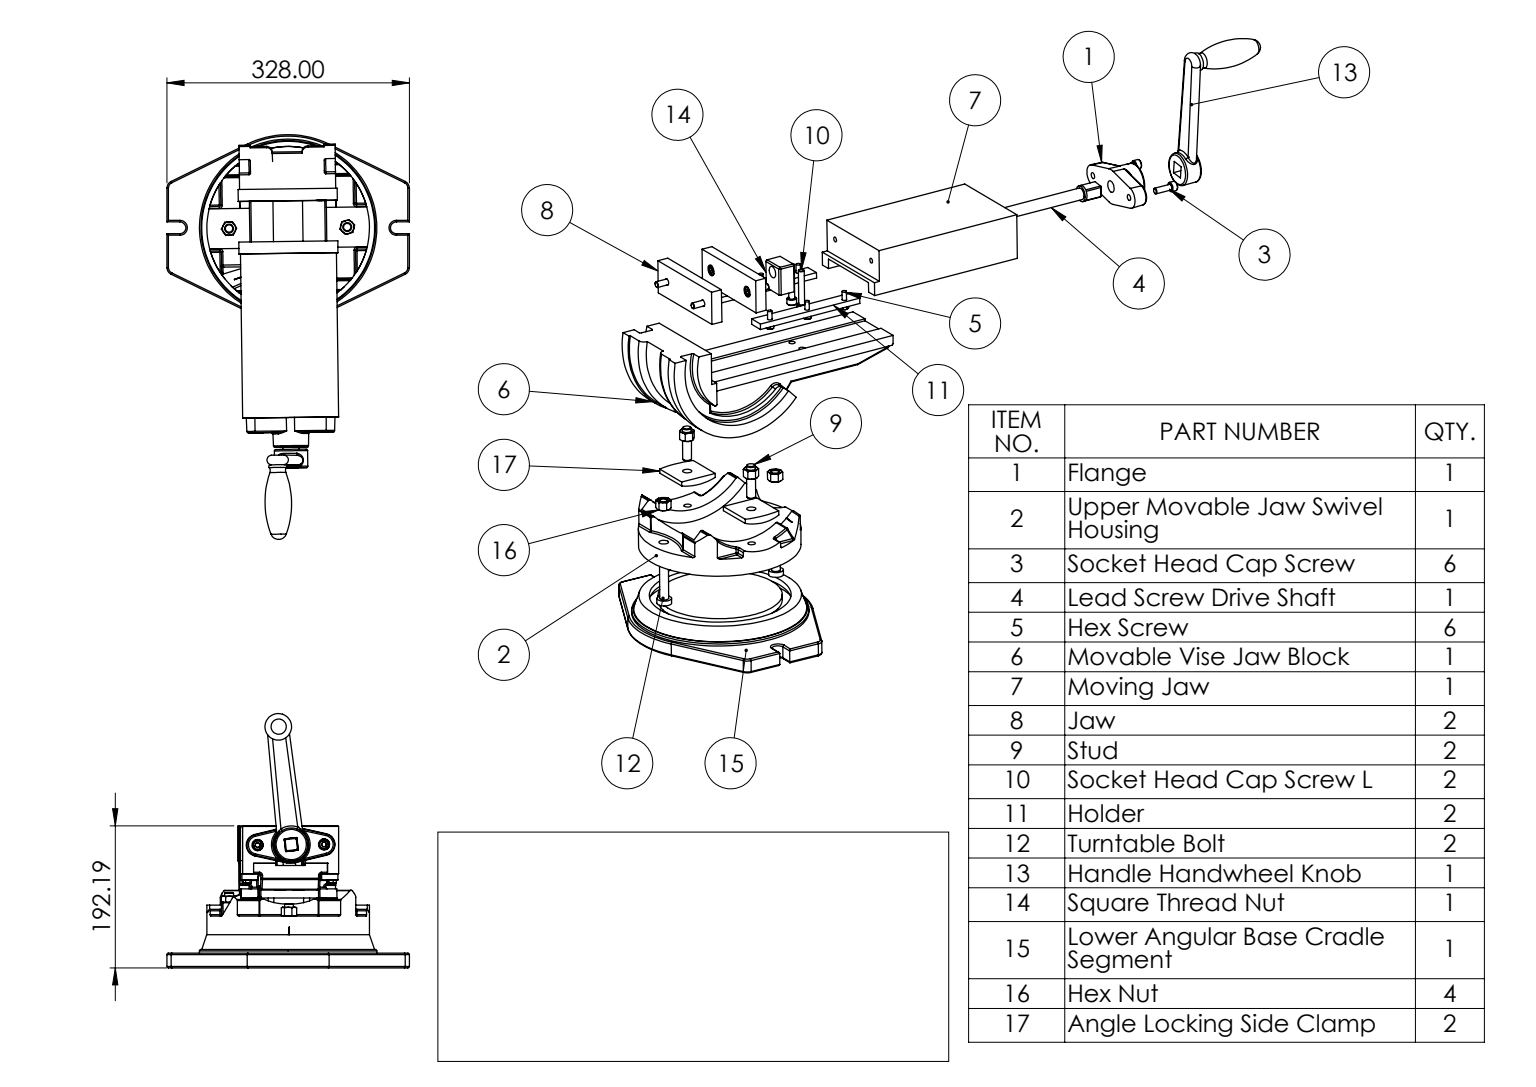
ISO-10303-21;
HEADER;
FILE_DESCRIPTION (('STEP AP214'),
    '1' );
FILE_NAME ('MAS-425',
    '2026-10-09T10:51:02',
    ( '' ),
    ( '' ),
    'SwSTEP 2.0',
    'SolidWorks 2026',
    '' );
FILE_SCHEMA (( 'AUTOMOTIVE_DESIGN' ));
ENDSEC;

DATA;
#1 = ORIENTED_EDGE ( 'NONE', *, *, #17423, .F. ) ;
#2 = EDGE_CURVE ( 'NONE', #15659, #11181, #7452, .T. ) ;
#3 = FACE_BOUND ( 'NONE', #13638, .T. ) ;
#4 = CARTESIAN_POINT ( 'NONE',  ( 8.705884045762138257, 173.3519990577861734, 81.47578913282544022 ) ) ;
#5 = EDGE_LOOP ( 'NONE', ( #8309, #15407, #11959, #15911 ) ) ;
#6 = CARTESIAN_POINT ( 'NONE',  ( -0.1662275214367944787, 327.2814318531398499, 311.3351636502816291 ) ) ;
#7 = LINE ( 'NONE', #21024, #14851 ) ;
#8 = ORIENTED_EDGE ( 'NONE', *, *, #1064, .F. ) ;
#9 = DIRECTION ( 'NONE',  ( 0.01292394549866739996, 0.005513023399721564584, 0.9999012842304692006 ) ) ;
#10 = CARTESIAN_POINT ( 'NONE',  ( -89.78468759032787716, 88.98018858692468314, 52.07678711320818365 ) ) ;
#11 = AXIS2_PLACEMENT_3D ( 'NONE', #11203, #9587, #5900 ) ;
#12 = VERTEX_POINT ( 'NONE', #2655 ) ;
#13 = VECTOR ( 'NONE', #9330, 999.9999999999998863 ) ;
#14 = ORIENTED_EDGE ( 'NONE', *, *, #14466, .T. ) ;
#15 = CARTESIAN_POINT ( 'NONE',  ( -41.94137166082473556, 162.5796238295972671, 273.2086669205137355 ) ) ;
#16 = CARTESIAN_POINT ( 'NONE',  ( -9.107733615807006800, 37.00000000000000711, -96.06569921463757566 ) ) ;
#17 = ORIENTED_EDGE ( 'NONE', *, *, #6536, .F. ) ;
#18 = AXIS2_PLACEMENT_3D ( 'NONE', #16748, #891, #15021 ) ;
#19 = CARTESIAN_POINT ( 'NONE',  ( 83.88156715903123484, 75.05939835648034375, 2.283427986461537440 ) ) ;
#20 = DIRECTION ( 'NONE',  ( 0.9999164797902017066, 6.965998958219365988E-18, -0.01292414190464157356 ) ) ;
#21 = EDGE_LOOP ( 'NONE', ( #14279, #17712, #11551, #2632 ) ) ;
#22 = AXIS2_PLACEMENT_3D ( 'NONE', #15032, #2937, #18572 ) ;
#23 = ORIENTED_EDGE ( 'NONE', *, *, #4860, .T. ) ;
#24 = DIRECTION ( 'NONE',  ( 0.9935244165829104634, 0.1136188085379686713, 0.000000000000000000 ) ) ;
#25 = CARTESIAN_POINT ( 'NONE',  ( -76.57490387278154742, 75.07748563434969924, 4.833641046600559044 ) ) ;
#26 = CARTESIAN_POINT ( 'NONE',  ( -10.01057122740781402, 165.1012737418342056, 308.8014639846969089 ) ) ;
#27 = EDGE_CURVE ( 'NONE', #4135, #17067, #5079, .T. ) ;
#28 = CARTESIAN_POINT ( 'NONE',  ( -105.7487010638476619, 78.91327849199103639, 30.28586431387788380 ) ) ;
#29 = EDGE_CURVE ( 'NONE', #2768, #16051, #13115, .T. ) ;
#30 = DIRECTION ( 'NONE',  ( 0.9909299940865187173, -0.1338359446631173233, -0.01207007604876291287 ) ) ;
#31 = CARTESIAN_POINT ( 'NONE',  ( -56.85751309718151703, 126.2713511641368171, 50.07958431720155090 ) ) ;
#32 = EDGE_CURVE ( 'NONE', #7434, #9119, #18827, .T. ) ;
#33 = AXIS2_PLACEMENT_3D ( 'NONE', #9862, #17006, #490 ) ;
#34 = DIRECTION ( 'NONE',  ( -7.125109674081160920E-05, 0.9999848031710253382, -0.005512562950849312846 ) ) ;
#35 = ORIENTED_EDGE ( 'NONE', *, *, #1256, .T. ) ;
#36 = VECTOR ( 'NONE', #11049, 1000.000000000000000 ) ;
#37 = DIRECTION ( 'NONE',  ( 6.641024085592512675E-15, -1.000000000000000000, 3.383900228611897455E-15 ) ) ;
#38 = ORIENTED_EDGE ( 'NONE', *, *, #21148, .T. ) ;
#39 = ORIENTED_EDGE ( 'NONE', *, *, #19350, .F. ) ;
#40 = UNCERTAINTY_MEASURE_WITH_UNIT (LENGTH_MEASURE( 1.000000000000000082E-05 ), #13566, 'distance_accuracy_value', 'NONE');
#41 = CARTESIAN_POINT ( 'NONE',  ( 15.61516006123881795, 188.4668067408832144, 308.5202341143809690 ) ) ;
#42 = AXIS2_PLACEMENT_3D ( 'NONE', #16731, #4517, #8084 ) ;
#43 = AXIS2_PLACEMENT_3D ( 'NONE', #10674, #12520, #10452 ) ;
#44 = VERTEX_POINT ( 'NONE', #20325 ) ;
#45 = DIRECTION ( 'NONE',  ( -0.7161863329816251511, -0.003898296230782347539, -0.6978982302147140881 ) ) ;
#46 = ADVANCED_BREP_SHAPE_REPRESENTATION ( '', ( #9964, #6292 ), #9601 ) ;
#47 = DIRECTION ( 'NONE',  ( 0.01292394549866738782, 0.005513023399720468239, 0.9999012842304692006 ) ) ;
#48 = CARTESIAN_POINT ( 'NONE',  ( -5.718390838975437873, 144.0378302125689629, 276.6767821598265300 ) ) ;
#49 = DIRECTION ( 'NONE',  ( -0.7944560844389300103, 0.000000000000000000, -0.6073216033519338586 ) ) ;
#50 = AXIS2_PLACEMENT_3D ( 'NONE', #20682, #18849, #13474 ) ;
#51 = CARTESIAN_POINT ( 'NONE',  ( -93.23587179807654479, 72.00000000000000000, -30.79757858250320979 ) ) ;
#52 = CARTESIAN_POINT ( 'NONE',  ( 13.04681478898882219, 190.3009582326741622, 320.8498813576193243 ) ) ;
#53 = CARTESIAN_POINT ( 'NONE',  ( 83.22761354253117361, 75.14843460673597519, -6.385946070498853544 ) ) ;
#54 = VECTOR ( 'NONE', #20690, 999.9999999999998863 ) ;
#55 = CARTESIAN_POINT ( 'NONE',  ( 19.35063451732290929, 183.1639393726175058, 309.5798762404240847 ) ) ;
#56 = CARTESIAN_POINT ( 'NONE',  ( -66.42677970909001317, 189.3893605493459233, -109.9672025422466959 ) ) ;
#57 = CARTESIAN_POINT ( 'NONE',  ( 1.364373935098378649E-14, 105.0000000000000000, -9.836450281572198869E-15 ) ) ;
#58 = EDGE_CURVE ( 'NONE', #6274, #3568, #1285, .T. ) ;
#59 = CARTESIAN_POINT ( 'NONE',  ( 93.17671387018316409, 79.04398536104964990, 26.22064129356684958 ) ) ;
#60 = SHAPE_REPRESENTATION_RELATIONSHIP ( 'NONE' , 'NONE' ,  #16508, #4953 ) ;
#61 = AXIS2_PLACEMENT_3D ( 'NONE', #18338, #21644, #15030 ) ;
#62 = EDGE_CURVE ( 'NONE', #12374, #18464, #11714, .T. ) ;
#63 = CARTESIAN_POINT ( 'NONE',  ( -8.812762866403248907, 186.1645115285507188, 321.8620257335252859 ) ) ;
#64 = DIRECTION ( 'NONE',  ( 0.9934404589540163366, 0.1135548637187051291, -0.01346653032743023830 ) ) ;
#65 = EDGE_LOOP ( 'NONE', ( #10795, #9717, #10945, #15498 ) ) ;
#67 = CARTESIAN_POINT ( 'NONE',  ( -92.91045972105430906, 79.04398536109844997, -26.22408268756080929 ) ) ;
#66 = VECTOR ( 'NONE', #9860, 1000.000000000000114 ) ;
#68 = EDGE_LOOP ( 'NONE', ( #15099, #11264, #5620 ) ) ;
#69 = VECTOR ( 'NONE', #9378, 999.9999999999998863 ) ;
#70 = VECTOR ( 'NONE', #5389, 1000.000000000000000 ) ;
#71 = CARTESIAN_POINT ( 'NONE',  ( -69.75324274910623501, 70.27959272172267902, -85.05633583411399457 ) ) ;
#72 = EDGE_CURVE ( 'NONE', #164, #20449, #17392, .T. ) ;
#73 = CARTESIAN_POINT ( 'NONE',  ( -37.87284078821844702, 165.3754468158257112, 244.8283704289042362 ) ) ;
#74 = ORIENTED_EDGE ( 'NONE', *, *, #20006, .F. ) ;
#75 = DIRECTION ( 'NONE',  ( 0.9999164797902018176, 2.001050586498093021E-22, -0.01292414190464117804 ) ) ;
#76 = CARTESIAN_POINT ( 'NONE',  ( 51.43549903698339421, 154.9275132768233618, 276.0443355225219761 ) ) ;
#77 = DIRECTION ( 'NONE',  ( 0.000000000000000000, 0.000000000000000000, -1.000000000000000000 ) ) ;
#78 = EDGE_CURVE ( 'NONE', #11089, #8677, #1606, .T. ) ;
#79 = ORIENTED_EDGE ( 'NONE', *, *, #13431, .F. ) ;
#80 = FACE_BOUND ( 'NONE', #4943, .T. ) ;
#81 = ORIENTED_EDGE ( 'NONE', *, *, #8487, .T. ) ;
#82 = AXIS2_PLACEMENT_3D ( 'NONE', #13509, #3038, #10060 ) ;
#83 = DIRECTION ( 'NONE',  ( 0.000000000000000000, -1.000000000000000000, 0.000000000000000000 ) ) ;
#84 = VECTOR ( 'NONE', #2049, 1000.000000000000114 ) ;
#85 = PRESENTATION_LAYER_ASSIGNMENT (  '', '', ( #9989 ) ) ;
#86 = CARTESIAN_POINT ( 'NONE',  ( 70.93357090261925180, 91.46354453597338363, 84.07396062241133450 ) ) ;
#87 = CARTESIAN_POINT ( 'NONE',  ( -8.855655583235034101, 185.7709171679380802, 321.2465429934534313 ) ) ;
#88 = DIRECTION ( 'NONE',  ( 0.000000000000000000, 1.000000000000000000, 0.000000000000000000 ) ) ;
#89 = LINE ( 'NONE', #16195, #5542 ) ;
#90 = ORIENTED_EDGE ( 'NONE', *, *, #19194, .F. ) ;
#91 = EDGE_CURVE ( 'NONE', #4221, #20506, #7354, .T. ) ;
#92 = DIRECTION ( 'NONE',  ( 0.9934404589540164476, 0.1135548637187057258, -0.01346653032743022095 ) ) ;
#93 = EDGE_CURVE ( 'NONE', #564, #16051, #11405, .T. ) ;
#94 = CARTESIAN_POINT ( 'NONE',  ( 87.98413419613014241, 100.6041916471018851, -66.02114910964037620 ) ) ;
#95 = CIRCLE ( 'NONE', #9269, 21.67179167071592261 ) ;
#96 = CARTESIAN_POINT ( 'NONE',  ( -45.67464185259402853, 168.2105890667581605, -51.90496219196452188 ) ) ;
#97 = CARTESIAN_POINT ( 'NONE',  ( -15.45047209318716419, 177.9595801977488634, 312.9923267615550344 ) ) ;
#98 = B_SPLINE_CURVE_WITH_KNOTS ( 'NONE', 3,
 ( #3660, #13798, #8829, #3553, #7001, #21013, #121, #3202 ),
 .UNSPECIFIED., .F., .F.,
 ( 4, 2, 2, 4 ),
 ( 0.005257893453559988640, 0.006567392922673305836, 0.007876892391786622163, 0.01049589133001326002 ),
 .UNSPECIFIED. ) ;
#99 = VERTEX_POINT ( 'NONE', #7105 ) ;
#100 = B_SPLINE_CURVE_WITH_KNOTS ( 'NONE', 3,
 ( #8667, #13977, #4769, #10088, #15381, #20512, #13534 ),
 .UNSPECIFIED., .F., .F.,
 ( 4, 3, 4 ),
 ( -5.915969516749687466E-08, 0.000000000000000000, 2.978207829266907417E-05 ),
 .UNSPECIFIED. ) ;
#101 = CARTESIAN_POINT ( 'NONE',  ( 17.83180013577688783, 184.4306634807684588, 307.6366520947308345 ) ) ;
#102 = CARTESIAN_POINT ( 'NONE',  ( -0.5772765004791020615, 70.09252763182293222, -80.84070517186570726 ) ) ;
#103 = DIRECTION ( 'NONE',  ( -7.125109674364536131E-05, 0.9999848031710253382, -0.005512562950849706628 ) ) ;
#104 = CIRCLE ( 'NONE', #1575, 11.00000000000000178 ) ;
#105 = CARTESIAN_POINT ( 'NONE',  ( -9.809641362382285124, 82.00000000000000000, -87.34492244913440118 ) ) ;
#106 = EDGE_CURVE ( 'NONE', #7605, #5654, #6985, .T. ) ;
#107 = ITEM_DEFINED_TRANSFORMATION ( 'NONE', 'NONE', #21637,  #6292 ) ;
#108 = DIRECTION ( 'NONE',  ( -0.9999164797902015955, 0.000000000000000000, 0.01292414190464162733 ) ) ;
#109 = DIRECTION ( 'NONE',  ( -0.01292394549866736179, -0.005513023399728320464, -0.9999012842304692006 ) ) ;
#110 = EDGE_CURVE ( 'NONE', #3828, #14649, #15744, .T. ) ;
#111 = CARTESIAN_POINT ( 'NONE',  ( 11.83347885643962982, 174.6861507205185546, 323.4518999165990181 ) ) ;
#112 = DIRECTION ( 'NONE',  ( 2.025474946048326158E-22, -1.000000000000000000, 1.876735158486679638E-22 ) ) ;
#113 = CONICAL_SURFACE ( 'NONE', #10017, 3.399999999999985700, 1.029744258676653201 ) ;
#114 = DIRECTION ( 'NONE',  ( -0.9999164797902015955, -2.001050586450178695E-22, 0.01292414190464131335 ) ) ;
#115 = ORIENTED_EDGE ( 'NONE', *, *, #3028, .T. ) ;
#116 = FACE_OUTER_BOUND ( 'NONE', #21594, .T. ) ;
#117 = CARTESIAN_POINT ( 'NONE',  ( -39.93340742419142941, 174.9483409995870886, 5.410635606648346752 ) ) ;
#118 = EDGE_LOOP ( 'NONE', ( #17233, #4566 ) ) ;
#119 = CARTESIAN_POINT ( 'NONE',  ( -49.95600144165727841, 95.32463374251413768, -43.99660977802226114 ) ) ;
#120 = EDGE_LOOP ( 'NONE', ( #22099, #16462, #18730 ) ) ;
#121 = CARTESIAN_POINT ( 'NONE',  ( -10.95382118728219289, 70.55908004698140701, -92.00507013140023105 ) ) ;
#122 = FACE_OUTER_BOUND ( 'NONE', #5169, .T. ) ;
#123 = AXIS2_PLACEMENT_3D ( 'NONE', #888, #21632, #12956 ) ;
#124 = CIRCLE ( 'NONE', #10026, 112.5000000000000142 ) ;
#125 = EDGE_CURVE ( 'NONE', #4735, #5612, #10337, .T. ) ;
#126 = VERTEX_POINT ( 'NONE', #10448 ) ;
#127 = FACE_BOUND ( 'NONE', #21151, .T. ) ;
#128 = CARTESIAN_POINT ( 'NONE',  ( 0.3194159855789066582, 327.3487718243365521, 314.2597695910868651 ) ) ;
#129 = EDGE_LOOP ( 'NONE', ( #6381, #6169 ) ) ;
#130 = AXIS2_PLACEMENT_3D ( 'NONE', #8032, #9876, #20201 ) ;
#131 = VECTOR ( 'NONE', #1451, 999.9999999999998863 ) ;
#132 = DIRECTION ( 'NONE',  ( 0.01292394549866738782, 0.005513023399720700692, 0.9999012842304693116 ) ) ;
#133 = CARTESIAN_POINT ( 'NONE',  ( -88.16866694100703228, 88.68864517119313007, 52.43947707082220688 ) ) ;
#135 = ORIENTED_EDGE ( 'NONE', *, *, #14584, .T. ) ;
#134 = VERTEX_POINT ( 'NONE', #1493 ) ;
#136 = AXIS2_PLACEMENT_3D ( 'NONE', #9103, #21501, #2221 ) ;
#137 = B_SPLINE_CURVE_WITH_KNOTS ( 'NONE', 3,
 ( #19717, #16214, #455, #4105, #14828, #14494 ),
 .UNSPECIFIED., .F., .F.,
 ( 4, 2, 4 ),
 ( 2.380730968138597170E-07, 0.002629065763328322300, 0.005257893453559830781 ),
 .UNSPECIFIED. ) ;
#138 = EDGE_CURVE ( 'NONE', #1183, #6442, #10411, .T. ) ;
#139 = ORIENTED_EDGE ( 'NONE', *, *, #21705, .T. ) ;
#140 = DIRECTION ( 'NONE',  ( 0.9999164797902015955, 6.965998958219364448E-18, -0.01292414190464157182 ) ) ;
#141 = CARTESIAN_POINT ( 'NONE',  ( 43.08423624159371457, 94.48610424851698042, 82.84014869562157912 ) ) ;
#142 = CARTESIAN_POINT ( 'NONE',  ( 80.59620023633263486, 75.13519862315604314, -6.109066223056235145 ) ) ;
#143 = CARTESIAN_POINT ( 'NONE',  ( -61.67972807482614428, 191.4143309225244707, 257.3032278304543183 ) ) ;
#144 = EDGE_LOOP ( 'NONE', ( #22040, #16025, #1524, #21274, #7268, #9424, #8449, #10368, #9326, #4340 ) ) ;
#145 = CARTESIAN_POINT ( 'NONE',  ( 20.36241020427591053, 184.0347753543214537, 278.2158687833080535 ) ) ;
#146 = ORIENTED_EDGE ( 'NONE', *, *, #11899, .T. ) ;
#147 = DIRECTION ( 'NONE',  ( 0.9909299940865187173, -0.1338359446631173233, -0.01207007604876291287 ) ) ;
#148 = CARTESIAN_POINT ( 'NONE',  ( -65.67129704762463405, 144.7109461922390778, -51.51693412452669918 ) ) ;
#149 = AXIS2_PLACEMENT_3D ( 'NONE', #2906, #22065, #6366 ) ;
#150 = DIRECTION ( 'NONE',  ( -7.125109674118361251E-05, 0.9999848031710253382, -0.005512562950849477644 ) ) ;
#151 = CIRCLE ( 'NONE', #6013, 2.499999999999988010 ) ;
#152 = CARTESIAN_POINT ( 'NONE',  ( -28.12186643111994044, 324.0859723387359850, 311.7141148554663914 ) ) ;
#153 = ORIENTED_EDGE ( 'NONE', *, *, #18129, .F. ) ;
#154 = PLANE ( 'NONE',  #20182 ) ;
#155 = EDGE_CURVE ( 'NONE', #11795, #1627, #509, .T. ) ;
#156 = CARTESIAN_POINT ( 'NONE',  ( -44.49054948644865703, 166.4747265717734308, 273.2201396957804036 ) ) ;
#157 = PLANE ( 'NONE',  #21075 ) ;
#158 = VECTOR ( 'NONE', #9778, 1000.000000000000000 ) ;
#159 = CARTESIAN_POINT ( 'NONE',  ( 105.4334892372614689, 71.72994009789539405, -31.36525700924963544 ) ) ;
#160 = VERTEX_POINT ( 'NONE', #21115 ) ;
#161 = AXIS2_PLACEMENT_3D ( 'NONE', #9912, #15227, #6474 ) ;
#162 = FACE_BOUND ( 'NONE', #20297, .T. ) ;
#163 = VERTEX_POINT ( 'NONE', #8594 ) ;
#164 = VERTEX_POINT ( 'NONE', #8472 ) ;
#165 = VERTEX_POINT ( 'NONE', #15520 ) ;
#166 = CARTESIAN_POINT ( 'NONE',  ( 14.63430001765469868, 189.2724070846429072, 308.1616490980433696 ) ) ;
#167 = VECTOR ( 'NONE', #3527, 999.9999999999998863 ) ;
#168 = VERTEX_POINT ( 'NONE', #19161 ) ;
#169 = EDGE_CURVE ( 'NONE', #21645, #1999, #4525, .T. ) ;
#170 = EDGE_CURVE ( 'NONE', #168, #18579, #18934, .T. ) ;
#171 = CARTESIAN_POINT ( 'NONE',  ( -90.06393689865117835, 72.00000000000000000, 59.85988923254397065 ) ) ;
#172 = EDGE_CURVE ( 'NONE', #2811, #3408, #19534, .T. ) ;
#173 = CARTESIAN_POINT ( 'NONE',  ( -14.82979117956944037, 177.4987173824078468, 90.64024647396865930 ) ) ;
#174 = AXIS2_PLACEMENT_3D ( 'NONE', #13516, #3386, #10402 ) ;
#175 = VECTOR ( 'NONE', #4968, 999.9999999999998863 ) ;
#176 = FACE_OUTER_BOUND ( 'NONE', #6477, .T. ) ;
#177 = CARTESIAN_POINT ( 'NONE',  ( 79.99331838321626265, 102.0000000000000000, -1.033931352371318058 ) ) ;
#178 = CARTESIAN_POINT ( 'NONE',  ( -38.71484115365228007, 95.23700578170286235, 83.13812943312275650 ) ) ;
#179 = CARTESIAN_POINT ( 'NONE',  ( -41.52755568966412625, 166.0426042274538077, 268.7837904884077034 ) ) ;
#180 = DIRECTION ( 'NONE',  ( 0.9999164797902017066, 2.045740421681430110E-15, -0.01292414190464156835 ) ) ;
#181 = CARTESIAN_POINT ( 'NONE',  ( 15.18113699892158763, 188.8369998821271452, 308.3433818295962396 ) ) ;
#182 = CARTESIAN_POINT ( 'NONE',  ( 92.53737097235195108, 79.85828562204582681, 28.87839056718317465 ) ) ;
#183 = DIRECTION ( 'NONE',  ( 7.125109674160325297E-05, -0.9999848031710252272, 0.005512562950849327591 ) ) ;
#184 = ORIENTED_EDGE ( 'NONE', *, *, #10599, .F. ) ;
#185 = CARTESIAN_POINT ( 'NONE',  ( -10.80196055862741211, 113.7230284608895943, 131.4548877534794542 ) ) ;
#186 = DIRECTION ( 'NONE',  ( -0.01292394549866750231, -0.005513023399722823126, -0.9999012842304692006 ) ) ;
#187 = ORIENTED_EDGE ( 'NONE', *, *, #11712, .T. ) ;
#188 = CARTESIAN_POINT ( 'NONE',  ( -92.67786813602107543, 77.16999450923083259, -28.87226322141232870 ) ) ;
#189 = ORIENTED_EDGE ( 'NONE', *, *, #8901, .F. ) ;
#190 = CIRCLE ( 'NONE', #9344, 2.000000000000000000 ) ;
#191 = CARTESIAN_POINT ( 'NONE',  ( 59.65023440614042727, 143.9188730675116688, 165.9879953250834603 ) ) ;
#192 = FACE_OUTER_BOUND ( 'NONE', #4432, .T. ) ;
#193 = CIRCLE ( 'NONE', #21802, 95.00000000000001421 ) ;
#194 = ORIENTED_EDGE ( 'NONE', *, *, #13859, .T. ) ;
#195 = DIRECTION ( 'NONE',  ( -0.9999164797902015955, -8.506845633049209592E-18, 0.01292414190464159611 ) ) ;
#196 = CARTESIAN_POINT ( 'NONE',  ( 45.44350069997184249, 168.6907664596096765, 34.02200722522287180 ) ) ;
#197 = CARTESIAN_POINT ( 'NONE',  ( 1.163172771417732010, 44.99899999999999523, 89.99248318111813205 ) ) ;
#198 = VERTEX_POINT ( 'NONE', #22578 ) ;
#199 = DIRECTION ( 'NONE',  ( 0.01292394549866734098, 0.005513023399720419666, 0.9999012842304692006 ) ) ;
#200 = ORIENTED_EDGE ( 'NONE', *, *, #18910, .T. ) ;
#201 = LINE ( 'NONE', #14344, #11898 ) ;
#202 = CARTESIAN_POINT ( 'NONE',  ( -39.36913080622078809, 72.00000000000000000, 87.51612159803859470 ) ) ;
#203 = CARTESIAN_POINT ( 'NONE',  ( -8.718981069309306164, 185.8769606721263017, 321.2367416126799640 ) ) ;
#204 = CARTESIAN_POINT ( 'NONE',  ( -90.61229378181283778, 77.84360403296375353, 32.30868923918552582 ) ) ;
#205 = PLANE ( 'NONE',  #10305 ) ;
#206 = ORIENTED_EDGE ( 'NONE', *, *, #693, .T. ) ;
#207 = CARTESIAN_POINT ( 'NONE',  ( -60.33297403592508346, 114.2134059809041418, 166.6289436847881689 ) ) ;
#208 = ADVANCED_FACE ( 'NONE', ( #17222 ), #15410, .F. ) ;
#209 = CARTESIAN_POINT ( 'NONE',  ( -16.46732747216173820, 164.3349221900030557, 301.8725943425079095 ) ) ;
#210 = CARTESIAN_POINT ( 'NONE',  ( 15.90349308958513141, 168.0612899129591824, 307.9342904543644863 ) ) ;
#211 = CARTESIAN_POINT ( 'NONE',  ( -13.46841022152523237, 180.7689078494431669, 321.2689861962914506 ) ) ;
#212 = AXIS2_PLACEMENT_3D ( 'NONE', #480, #21365, #21476 ) ;
#213 = CARTESIAN_POINT ( 'NONE',  ( 20.69445389845595784, 181.8968845288082434, 314.6913679966366999 ) ) ;
#214 = EDGE_LOOP ( 'NONE', ( #14788, #8184, #10598, #16060, #20937 ) ) ;
#215 = ADVANCED_FACE ( 'NONE', ( #14014 ), #12056, .T. ) ;
#216 = DIRECTION ( 'NONE',  ( 0.000000000000000000, 1.000000000000000000, -0.000000000000000000 ) ) ;
#217 = CONTEXT_DEPENDENT_SHAPE_REPRESENTATION ( #13531, #16900 ) ;
#218 = CARTESIAN_POINT ( 'NONE',  ( 36.24790013166018099, 94.37751527644310556, 82.16087381192814121 ) ) ;
#219 = EDGE_CURVE ( 'NONE', #11742, #21224, #10193, .T. ) ;
#220 = EDGE_CURVE ( 'NONE', #18203, #7136, #3541, .T. ) ;
#221 = CARTESIAN_POINT ( 'NONE',  ( -17.10066205189340849, 316.2389990861104820, 322.8183011548654804 ) ) ;
#222 = CYLINDRICAL_SURFACE ( 'NONE', #2944, 2.000000000000001776 ) ;
#223 = DIRECTION ( 'NONE',  ( 0.9232306267972774094, 0.000000000000000000, -0.3842462878721227826 ) ) ;
#224 = EDGE_LOOP ( 'NONE', ( #13231, #22623, #16630, #19910 ) ) ;
#225 = EDGE_LOOP ( 'NONE', ( #13563, #14195, #15245 ) ) ;
#226 = CARTESIAN_POINT ( 'NONE',  ( -41.56623493000981284, 72.00000000000000000, -82.46967996629571473 ) ) ;
#227 = PRODUCT_DEFINITION_SHAPE ( 'NONE', 'NONE',  #22690 ) ;
#228 = CARTESIAN_POINT ( 'NONE',  ( -1.163172771417702700, 69.99999999999998579, -89.99248318111824574 ) ) ;
#229 = ORIENTED_EDGE ( 'NONE', *, *, #7447, .T. ) ;
#230 = CARTESIAN_POINT ( 'NONE',  ( 39.42082737383937996, 91.17157287525387233, -83.51645567887783272 ) ) ;
#231 = ORIENTED_EDGE ( 'NONE', *, *, #5950, .F. ) ;
#232 = CARTESIAN_POINT ( 'NONE',  ( 106.2491592972476298, 77.90302844854615216, 28.48020057081471279 ) ) ;
#233 = DIRECTION ( 'NONE',  ( -0.9232306267972774094, 0.000000000000000000, 0.3842462878721227826 ) ) ;
#234 = DIRECTION ( 'NONE',  ( -0.01292394549866745720, -0.005513023399720816918, -0.9999012842304692006 ) ) ;
#235 = EDGE_CURVE ( 'NONE', #9934, #22618, #12029, .T. ) ;
#236 = EDGE_LOOP ( 'NONE', ( #19815, #2984, #795, #12420, #9588 ) ) ;
#237 = DIRECTION ( 'NONE',  ( 0.000000000000000000, 0.000000000000000000, 1.000000000000000000 ) ) ;
#238 = DIRECTION ( 'NONE',  ( 0.01246513159389400598, 0.2641402835564878870, 0.9644037178988087433 ) ) ;
#239 = CARTESIAN_POINT ( 'NONE',  ( 21.90287145686899706, 168.7773271647431841, 315.3565719312696842 ) ) ;
#240 = EDGE_CURVE ( 'NONE', #22376, #21368, #5043, .T. ) ;
#241 = ORIENTED_EDGE ( 'NONE', *, *, #10232, .T. ) ;
#242 = CARTESIAN_POINT ( 'NONE',  ( -29.42617654240078551, 169.3906321239456361, -110.1596432836334856 ) ) ;
#243 = CARTESIAN_POINT ( 'NONE',  ( -89.64611244253616462, 89.06139627483084098, 51.86061978640490366 ) ) ;
#244 = ADVANCED_FACE ( 'NONE', ( #2899 ), #1200, .F. ) ;
#246 = ORIENTED_EDGE ( 'NONE', *, *, #15979, .F. ) ;
#245 = ORIENTED_EDGE ( 'NONE', *, *, #7257, .T. ) ;
#247 = EDGE_CURVE ( 'NONE', #11011, #13307, #20124, .T. ) ;
#248 = ORIENTED_EDGE ( 'NONE', *, *, #8242, .F. ) ;
#249 = DIRECTION ( 'NONE',  ( 0.3101392564284310427, 0.9506461370142480494, -0.009250070373107139796 ) ) ;
#250 = DIRECTION ( 'NONE',  ( 0.01292394549866731669, 0.005513023399720593139, 0.9999012842304692006 ) ) ;
#251 = VERTEX_POINT ( 'NONE', #22395 ) ;
#252 = CARTESIAN_POINT ( 'NONE',  ( 11.11764968563295142, 180.4772689128618879, 86.40582449793498654 ) ) ;
#253 = CARTESIAN_POINT ( 'NONE',  ( -90.15100670864553933, 87.99029836822313655, 53.12346227685477373 ) ) ;
#254 = LINE ( 'NONE', #14055, #10043 ) ;
#255 = ORIENTED_EDGE ( 'NONE', *, *, #12322, .T. ) ;
#256 = CARTESIAN_POINT ( 'NONE',  ( 48.39260390757410590, 174.4164586986524057, 267.9754221921975272 ) ) ;
#257 = ORIENTED_EDGE ( 'NONE', *, *, #16631, .F. ) ;
#258 = CARTESIAN_POINT ( 'NONE',  ( 79.99331838321626265, 54.99999999999999289, -1.033931352371318058 ) ) ;
#259 = DIRECTION ( 'NONE',  ( -0.000000000000000000, -1.000000000000000000, -0.000000000000000000 ) ) ;
#260 = DIRECTION ( 'NONE',  ( -0.9934404589540163366, -0.1135548637187053511, 0.01346653032743023309 ) ) ;
#261 = CARTESIAN_POINT ( 'NONE',  ( -28.28143568398816399, 324.0695986473149901, 312.1786345499324398 ) ) ;
#262 = DIRECTION ( 'NONE',  ( -0.01292394549866739996, -0.005513023399721131770, -0.9999012842304692006 ) ) ;
#263 = CARTESIAN_POINT ( 'NONE',  ( -39.11958398656035030, 107.9174803907495885, 72.42004164600064087 ) ) ;
#264 = DIRECTION ( 'NONE',  ( -7.125109674159588039E-05, 0.9999848031710253382, -0.005512562950848870491 ) ) ;
#265 = CARTESIAN_POINT ( 'NONE',  ( 105.3069082217399597, 70.76149960027359498, -31.78775043357529739 ) ) ;
#266 = ORIENTED_EDGE ( 'NONE', *, *, #3629, .T. ) ;
#267 = ADVANCED_FACE ( 'NONE', ( #15553 ), #14170, .F. ) ;
#268 = DIRECTION ( 'NONE',  ( 0.9232306267972772984, 0.000000000000000000, -0.3842462878721232822 ) ) ;
#269 = EDGE_LOOP ( 'NONE', ( #10049, #17678 ) ) ;
#270 = ORIENTED_EDGE ( 'NONE', *, *, #14726, .F. ) ;
#271 = EDGE_LOOP ( 'NONE', ( #6417, #19362, #17256, #12411 ) ) ;
#272 = UNCERTAINTY_MEASURE_WITH_UNIT (LENGTH_MEASURE( 1.000000000000000082E-05 ), #22042, 'distance_accuracy_value', 'NONE');
#273 = CARTESIAN_POINT ( 'NONE',  ( 19.91213793988244163, 183.5619383714575861, 314.9323046934921422 ) ) ;
#274 = ORIENTED_EDGE ( 'NONE', *, *, #11916, .F. ) ;
#275 = ADVANCED_FACE ( 'NONE', ( #19418 ), #17495, .F. ) ;
#276 = FACE_OUTER_BOUND ( 'NONE', #812, .T. ) ;
#277 = DIRECTION ( 'NONE',  ( 0.9999164797902017066, 2.001050586450178931E-22, -0.01292414190464131508 ) ) ;
#278 = CARTESIAN_POINT ( 'NONE',  ( -91.88175745861167343, 69.99999999999998579, 60.48014731673399069 ) ) ;
#279 = FACE_BOUND ( 'NONE', #1045, .T. ) ;
#280 = CARTESIAN_POINT ( 'NONE',  ( -38.57134427488318806, 95.07266577213218284, 83.30245068639356987 ) ) ;
#281 = DIRECTION ( 'NONE',  ( -0.01292394549866733230, -0.005513023399720419666, -0.9999012842304692006 ) ) ;
#282 = CARTESIAN_POINT ( 'NONE',  ( 76.11837255219295173, 75.12984171660241373, -5.954615140807677953 ) ) ;
#283 = CARTESIAN_POINT ( 'NONE',  ( 19.70626577706693894, 182.8347090725441433, 310.2503944804881826 ) ) ;
#284 = CARTESIAN_POINT ( 'NONE',  ( 90.70439626174579928, 79.29995750804924626, 27.08818539008225912 ) ) ;
#285 = CARTESIAN_POINT ( 'NONE',  ( 90.15711184568685610, 79.46353706204938305, 27.61532001585838714 ) ) ;
#286 = ORIENTED_EDGE ( 'NONE', *, *, #7951, .T. ) ;
#287 =( NAMED_UNIT ( * ) SI_UNIT ( $, .STERADIAN. ) SOLID_ANGLE_UNIT ( ) );
#288 = CIRCLE ( 'NONE', #22624, 0.009999999999999205705 ) ;
#289 = ADVANCED_FACE ( 'NONE', ( #16063 ), #9015, .T. ) ;
#290 = CARTESIAN_POINT ( 'NONE',  ( -9.470826101554981946, 187.1917151187963384, 321.2300099800097541 ) ) ;
#291 = DIRECTION ( 'NONE',  ( 7.125109674160258889E-05, -0.9999848031710252272, 0.005512562950849897447 ) ) ;
#292 = EDGE_CURVE ( 'NONE', #16435, #21883, #7077, .T. ) ;
#293 = ORIENTED_EDGE ( 'NONE', *, *, #12181, .F. ) ;
#294 = DIRECTION ( 'NONE',  ( 0.7069973413461587697, 0.7070960354057281849, -0.01303671902605322945 ) ) ;
#295 = EDGE_LOOP ( 'NONE', ( #16677, #766, #19558, #3200 ) ) ;
#296 = B_SPLINE_CURVE_WITH_KNOTS ( 'NONE', 3,
 ( #20681, #1405, #18731, #13805, #4936, #18621, #1059, #11969, #4819, #17038, #18953, #20788, #17137, #20446, #8179, #13473 ),
 .UNSPECIFIED., .F., .F.,
 ( 4, 2, 2, 2, 2, 2, 2, 4 ),
 ( 0.000000000000000000, 0.0008474927940828290429, 0.001271239191124224699, 0.001694985588165620572, 0.002118731985207016229, 0.002542478382248412102, 0.002966224779289807541, 0.003389971176331203415 ),
 .UNSPECIFIED. ) ;
#297 = VECTOR ( 'NONE', #9208, 1000.000000000000114 ) ;
#298 = EDGE_LOOP ( 'NONE', ( #1646, #5855, #3036, #20103 ) ) ;
#299 = CARTESIAN_POINT ( 'NONE',  ( -5.672696058028124710, 81.44153265534504271, -98.91173476717540325 ) ) ;
#300 = CARTESIAN_POINT ( 'NONE',  ( -1.163172771417702700, 81.97459999999998104, -89.99248318111824574 ) ) ;
#301 = EDGE_LOOP ( 'NONE', ( #15173, #17120, #19580, #5311 ) ) ;
#302 = DIRECTION ( 'NONE',  ( 0.01292394549866740169, 0.005513023399720822990, 0.9999012842304693116 ) ) ;
#303 = VECTOR ( 'NONE', #7071, 999.9999999999998863 ) ;
#304 =( REPRESENTATION_RELATIONSHIP ('NONE','NONE', #11808, #10922 ) REPRESENTATION_RELATIONSHIP_WITH_TRANSFORMATION ( #3089 )SHAPE_REPRESENTATION_RELATIONSHIP( ) );
#305 = DIRECTION ( 'NONE',  ( 0.9506032891036977350, -0.3102281881984299550, -0.01057629388543066158 ) ) ;
#306 = B_SPLINE_CURVE_WITH_KNOTS ( 'NONE', 3,
 ( #21331, #5362, #6982, #1942, #105, #14363 ),
 .UNSPECIFIED., .F., .F.,
 ( 4, 2, 4 ),
 ( 0.009270618776430233909, 0.01189894710419334665, 0.01452727543195645940 ),
 .UNSPECIFIED. ) ;
#307 = VERTEX_POINT ( 'NONE', #5575 ) ;
#308 = CARTESIAN_POINT ( 'NONE',  ( -22.02882225528089322, 319.7347194434814242, 320.5895957426023415 ) ) ;
#309 = VERTEX_POINT ( 'NONE', #21424 ) ;
#310 = CARTESIAN_POINT ( 'NONE',  ( -55.33894950108835076, 126.9191314136037789, 167.5679852142818334 ) ) ;
#311 = DIRECTION ( 'NONE',  ( 0.01292394549866739996, 0.005513023399721131770, 0.9999012842304692006 ) ) ;
#312 = EDGE_LOOP ( 'NONE', ( #22638, #21700, #16864 ) ) ;
#313 = CARTESIAN_POINT ( 'NONE',  ( -10.06383400738342360, 187.4687485412983108, 321.1393786276795481 ) ) ;
#314 = CARTESIAN_POINT ( 'NONE',  ( -91.08520856931303911, 77.44390114805533187, 31.69197020849769686 ) ) ;
#315 = CARTESIAN_POINT ( 'NONE',  ( 67.23655452815148692, 145.1029152106949027, 17.86880078497820179 ) ) ;
#316 = ORIENTED_EDGE ( 'NONE', *, *, #15570, .F. ) ;
#317 = TOROIDAL_SURFACE ( 'NONE', #19007, 12.37020706055087516, 2.000000000000000000 ) ;
#318 = CARTESIAN_POINT ( 'NONE',  ( -13.33381189847107784, 183.5857969768588589, 309.7596506135559480 ) ) ;
#319 = ADVANCED_FACE ( 'NONE', ( #17546 ), #8781, .T. ) ;
#320 = CARTESIAN_POINT ( 'NONE',  ( -41.47069032946998846, 166.0668615304125808, 273.1833561390217824 ) ) ;
#321 = AXIS2_PLACEMENT_3D ( 'NONE', #22086, #7878, #10397 ) ;
#322 = CARTESIAN_POINT ( 'NONE',  ( 18.31365161534814945, 168.3394720871181960, 308.5681747117120608 ) ) ;
#323 = CARTESIAN_POINT ( 'NONE',  ( -14.60451153091767118, 179.2935387600311401, 317.4001766113444774 ) ) ;
#324 = ORIENTED_EDGE ( 'NONE', *, *, #12603, .F. ) ;
#325 = DIRECTION ( 'NONE',  ( 0.01292414190464174703, 0.000000000000000000, 0.9999164797902015955 ) ) ;
#326 =( BOUNDED_SURFACE ( )  B_SPLINE_SURFACE ( 3, 2, ( 
 ( #2487, #894, #11567 ),
 ( #1117, #14687, #22097 ),
 ( #11112, #18134, #9486 ),
 ( #2827, #8113, #7770 ),
 ( #14809, #13081, #4304 ),
 ( #11333, #16646, #14924 ),
 ( #998, #21864, #6160 ),
 ( #13185, #2385, #20151 ),
 ( #18461, #2723, #4540 ),
 ( #9377, #16853, #16751 ),
 ( #15145, #7985, #15025 ),
 ( #21979, #6279, #13305 ),
 ( #6398, #19810, #16411 ),
 ( #10404, #6504, #1347 ),
 ( #4752, #11794, #13518 ),
 ( #6725, #18893, #10288 ),
 ( #3156, #15697, #11911 ),
 ( #15366, #3390, #10171 ) ),
 .UNSPECIFIED., .F., .F., .T. ) 
 B_SPLINE_SURFACE_WITH_KNOTS ( ( 4, 2, 2, 2, 2, 2, 2, 2, 4 ),
 ( 3, 3 ),
 ( 0.002597246120634449582, 0.003399884678228176898, 0.004202523235821904214, 0.005005161793415631097, 0.005807800351009358847, 0.006610438908603086597, 0.007413077466196813479, 0.008215716023790540362, 0.009018354581384268112 ),
 ( 0.000000000000000000, 1.000000000000000000 ),
 .UNSPECIFIED. ) 
 GEOMETRIC_REPRESENTATION_ITEM ( )  RATIONAL_B_SPLINE_SURFACE ( (
 ( 1.000000000000000000, 0.5963808372950818448, 1.000000000000000000),
 ( 1.000000000000000000, 0.5963839598475944026, 1.000000000000000000),
 ( 1.000000000000000000, 0.5970886094881097117, 1.000000000000000000),
 ( 1.000000000000000000, 0.5998681984912884735, 1.000000000000000000),
 ( 1.000000000000000000, 0.6019790828716350406, 1.000000000000000000),
 ( 1.000000000000000000, 0.6074656362385489894, 1.000000000000000000),
 ( 1.000000000000000000, 0.6108290540004600588, 1.000000000000000000),
 ( 1.000000000000000000, 0.6188252630046860991, 1.000000000000000000),
 ( 1.000000000000000000, 0.6234423941984682527, 1.000000000000000000),
 ( 1.000000000000000000, 0.6335838931037546251, 1.000000000000000000),
 ( 1.000000000000000000, 0.6391861101558512503, 1.000000000000000000),
 ( 1.000000000000000000, 0.6512661799274815921, 1.000000000000000000),
 ( 1.000000000000000000, 0.6576333021889211317, 1.000000000000000000),
 ( 1.000000000000000000, 0.6710088154584188391, 1.000000000000000000),
 ( 1.000000000000000000, 0.6780884601156443869, 1.000000000000000000),
 ( 1.000000000000000000, 0.6924279500034885571, 1.000000000000000000),
 ( 1.000000000000000000, 0.6997125326201816264, 1.000000000000000000),
 ( 1.000000000000000000, 0.7071067811865476838, 1.000000000000000000) ) ) 
 REPRESENTATION_ITEM ( '' )  SURFACE ( )  );
#327 = ORIENTED_EDGE ( 'NONE', *, *, #6954, .T. ) ;
#328 = CARTESIAN_POINT ( 'NONE',  ( 11.85964614693714836, 187.7423844643599296, 304.8777488482054423 ) ) ;
#329 = CIRCLE ( 'NONE', #7287, 112.5000000000000284 ) ;
#330 = CARTESIAN_POINT ( 'NONE',  ( -9.841028579513169561, 187.8130746588807938, 321.1594247271215750 ) ) ;
#331 = DIRECTION ( 'NONE',  ( 2.025474946048326158E-22, -1.000000000000000000, 1.876735158486679638E-22 ) ) ;
#332 = VECTOR ( 'NONE', #8959, 1000.000000000000114 ) ;
#333 = DIRECTION ( 'NONE',  ( -0.7070981056135049458, 0.7070960354057279629, 0.005240777737525892203 ) ) ;
#334 = ORIENTED_EDGE ( 'NONE', *, *, #20168, .F. ) ;
#335 = CARTESIAN_POINT ( 'NONE',  ( -66.44851505496320954, 169.3797848675314128, -111.6488252521261160 ) ) ;
#336 = LINE ( 'NONE', #12856, #8327 ) ;
#337 = ORIENTED_EDGE ( 'NONE', *, *, #2949, .T. ) ;
#338 = CARTESIAN_POINT ( 'NONE',  ( -50.59154831888564274, 96.21415597129798414, -45.44386052779758245 ) ) ;
#339 = ORIENTED_EDGE ( 'NONE', *, *, #11190, .F. ) ;
#340 = CARTESIAN_POINT ( 'NONE',  ( -48.94038278341281512, 95.51270090492249665, 82.30370228625183415 ) ) ;
#341 = DIRECTION ( 'NONE',  ( 0.01292394549866738782, 0.005513023399720700692, 0.9999012842304693116 ) ) ;
#342 = DIRECTION ( 'NONE',  ( 0.3101392564284315978, 0.9506461370142478273, -0.009250070373107145000 ) ) ;
#343 = CARTESIAN_POINT ( 'NONE',  ( 11.77442667496907625, 158.9997348699313591, 299.5367818821357560 ) ) ;
#344 = ORIENTED_EDGE ( 'NONE', *, *, #10316, .T. ) ;
#345 = VERTEX_POINT ( 'NONE', #76 ) ;
#346 = CARTESIAN_POINT ( 'NONE',  ( 40.57355171551004958, 108.0982075334647163, 198.8652726751216449 ) ) ;
#347 = CLOSED_SHELL ( 'NONE', ( #16015, #16676, #7875, #358, #5419, #11925, #2214, #215, #20046 ) ) ;
#348 = AXIS2_PLACEMENT_3D ( 'NONE', #1799, #199, #10640 ) ;
#349 = EDGE_CURVE ( 'NONE', #12132, #16568, #18988, .T. ) ;
#350 = CARTESIAN_POINT ( 'NONE',  ( 0.2417370086904135351, 327.3338204178164688, 312.7560729848880214 ) ) ;
#351 = CIRCLE ( 'NONE', #15405, 6.500000000000013323 ) ;
#352 = EDGE_LOOP ( 'NONE', ( #16374, #6015 ) ) ;
#353 = CARTESIAN_POINT ( 'NONE',  ( -42.64894290516974706, 118.1474297122749135, 27.43850586800562752 ) ) ;
#354 = CARTESIAN_POINT ( 'NONE',  ( -89.81089220510853011, 88.95379388444949598, 52.12444704693557895 ) ) ;
#355 = SHAPE_DEFINITION_REPRESENTATION ( #14203, #21889 ) ;
#357 = ORIENTED_EDGE ( 'NONE', *, *, #20567, .F. ) ;
#356 = ORIENTED_EDGE ( 'NONE', *, *, #20168, .T. ) ;
#358 = ADVANCED_FACE ( 'NONE', ( #21968 ), #16637, .T. ) ;
#359 = ORIENTED_EDGE ( 'NONE', *, *, #12423, .F. ) ;
#360 = CARTESIAN_POINT ( 'NONE',  ( -12.86548928906161571, 326.2291019854885121, 410.4442357137708086 ) ) ;
#361 = CARTESIAN_POINT ( 'NONE',  ( -44.25520882077128704, 168.2183454221810734, 273.2074843050344271 ) ) ;
#362 = EDGE_LOOP ( 'NONE', ( #12674, #9127, #10341, #20941, #20495 ) ) ;
#363 = AXIS2_PLACEMENT_3D ( 'NONE', #1584, #20516, #11935 ) ;
#364 = DIRECTION ( 'NONE',  ( -0.000000000000000000, -1.000000000000000000, 0.000000000000000000 ) ) ;
#365 = MECHANICAL_DESIGN_GEOMETRIC_PRESENTATION_REPRESENTATION (  '', ( #14686 ), #5105 ) ;
#366 = DIRECTION ( 'NONE',  ( 7.125109674403838460E-05, -0.9999848031710253382, 0.005512562950847868688 ) ) ;
#367 = VERTEX_POINT ( 'NONE', #15252 ) ;
#368 = EDGE_CURVE ( 'NONE', #10057, #21384, #12802, .T. ) ;
#369 = VERTEX_POINT ( 'NONE', #17174 ) ;
#370 = AXIS2_PLACEMENT_3D ( 'NONE', #9762, #6313, #11942 ) ;
#371 = CARTESIAN_POINT ( 'NONE',  ( -93.21002351426726307, 77.12912189496638860, -28.79774562292281104 ) ) ;
#372 = CARTESIAN_POINT ( 'NONE',  ( -24.73308955485819283, 324.4589790655039110, 308.1131263010046837 ) ) ;
#373 = CARTESIAN_POINT ( 'NONE',  ( 50.34271970654513950, 126.1473081376433214, 26.19246016726700788 ) ) ;
#374 = CYLINDRICAL_SURFACE ( 'NONE', #1941, 2.000000000000001332 ) ;
#375 = DIRECTION ( 'NONE',  ( 0.01292394549866743812, 0.005513023399720639109, 0.9999012842304693116 ) ) ;
#376 = AXIS2_PLACEMENT_3D ( 'NONE', #2393, #7090, #10992 ) ;
#377 = CYLINDRICAL_SURFACE ( 'NONE', #4764, 2.499999999999988010 ) ;
#378 = ADVANCED_FACE ( 'NONE', ( #6928 ), #5321, .T. ) ;
#379 = VERTEX_POINT ( 'NONE', #17766 ) ;
#380 = EDGE_CURVE ( 'NONE', #16237, #5742, #16043, .T. ) ;
#381 = DIRECTION ( 'NONE',  ( 7.125109674160258889E-05, -0.9999848031710252272, 0.005512562950849897447 ) ) ;
#382 = ORIENTED_EDGE ( 'NONE', *, *, #15008, .F. ) ;
#383 = CARTESIAN_POINT ( 'NONE',  ( -1.163172771417702700, 81.34441321561124028, -89.99248318111824574 ) ) ;
#384 = VECTOR ( 'NONE', #9453, 1000.000000000000000 ) ;
#385 = CARTESIAN_POINT ( 'NONE',  ( 19.41596747074044060, 184.3392198334767329, 316.6735434663280557 ) ) ;
#386 = AXIS2_PLACEMENT_3D ( 'NONE', #18232, #2255, #768 ) ;
#387 = ORIENTED_EDGE ( 'NONE', *, *, #12460, .T. ) ;
#388 = EDGE_CURVE ( 'NONE', #8063, #7165, #5071, .T. ) ;
#389 = AXIS2_PLACEMENT_3D ( 'NONE', #2582, #21844, #9353 ) ;
#390 = DIRECTION ( 'NONE',  ( 0.01292414190464223969, 1.902755938799532355E-22, 0.9999164797902017066 ) ) ;
#391 = DIRECTION ( 'NONE',  ( -0.3796287383013210448, 0.9251388995215469313, -0.0001940304313831171454 ) ) ;
#392 = CARTESIAN_POINT ( 'NONE',  ( 91.23603883849617091, 72.00000000000000000, 30.82342686631245243 ) ) ;
#393 = CARTESIAN_POINT ( 'NONE',  ( -36.73936676148915126, 94.93197183469659706, -81.60001862646660697 ) ) ;
#394 = DIRECTION ( 'NONE',  ( 0.000000000000000000, -0.000000000000000000, 1.000000000000000000 ) ) ;
#395 = CARTESIAN_POINT ( 'NONE',  ( -38.29718547875438617, 94.85299739018206822, 83.52102959496109236 ) ) ;
#396 = EDGE_CURVE ( 'NONE', #4308, #9861, #9699, .T. ) ;
#397 = CARTESIAN_POINT ( 'NONE',  ( 106.2089377515399065, 34.61572286322119396, 28.62973177816241588 ) ) ;
#398 = CARTESIAN_POINT ( 'NONE',  ( 79.50704247290580895, 75.20582465103802861, -7.278313778469502893 ) ) ;
#399 = CARTESIAN_POINT ( 'NONE',  ( 19.45541216839452048, 183.1297393420369417, 311.7642400163919660 ) ) ;
#400 = CARTESIAN_POINT ( 'NONE',  ( 89.22767861003023881, 80.31838830481380853, 30.18953644180654550 ) ) ;
#401 = CIRCLE ( 'NONE', #33, 1.999999999999997780 ) ;
#402 = VECTOR ( 'NONE', #14560, 999.9999999999998863 ) ;
#403 = CARTESIAN_POINT ( 'NONE',  ( 90.51972003054841309, 79.34791451281842001, 27.24428967784124822 ) ) ;
#404 = CYLINDRICAL_SURFACE ( 'NONE', #18670, 2.499999999999988010 ) ;
#405 = CARTESIAN_POINT ( 'NONE',  ( -90.43474204040838060, 34.61572286322119396, 31.17139488067998343 ) ) ;
#406 = EDGE_CURVE ( 'NONE', #20552, #2150, #13382, .T. ) ;
#407 = ADVANCED_FACE ( 'NONE', ( #8297 ), #9856, .T. ) ;
#408 = CARTESIAN_POINT ( 'NONE',  ( -8.586490856789254167, 185.8024398487989686, 322.3033838124611634 ) ) ;
#409 = CONICAL_SURFACE ( 'NONE', #3707, 9.000000000000001776, 1.047197551196594301 ) ;
#410 = PLANE ( 'NONE',  #2962 ) ;
#411 = ORIENTED_EDGE ( 'NONE', *, *, #12797, .F. ) ;
#412 = CARTESIAN_POINT ( 'NONE',  ( -92.63973831233892042, 79.05196971970110553, -26.25410855708505409 ) ) ;
#413 = ORIENTED_EDGE ( 'NONE', *, *, #15984, .T. ) ;
#414 = CIRCLE ( 'NONE', #19108, 7.500000000000002665 ) ;
#415 = DIRECTION ( 'NONE',  ( 0.01292394549866743812, 0.005513023399720639109, 0.9999012842304693116 ) ) ;
#416 = VECTOR ( 'NONE', #1504, 1000.000000000000000 ) ;
#417 = DIRECTION ( 'NONE',  ( 0.01292394549866731669, 0.005513023399720593139, 0.9999012842304692006 ) ) ;
#418 = CIRCLE ( 'NONE', #14381, 0.3999999999999986899 ) ;
#419 = DIRECTION ( 'NONE',  ( 0.01292414190464174703, 0.000000000000000000, 0.9999164797902015955 ) ) ;
#420 = DIRECTION ( 'NONE',  ( -7.125109674025824596E-05, 0.9999848031710253382, -0.005512562950848693549 ) ) ;
#421 = B_SPLINE_CURVE_WITH_KNOTS ( 'NONE', 3,
 ( #14409, #16130, #12222, #12679, #7032, #7150, #17960, #15907, #14177, #10490, #10589, #5523, #10835, #2094, #19205, #17501, #21045, #3916, #2196, #14060, #5402, #19548, #5298, #3815, #12338, #1753, #8731, #9199, #15785, #25, #12439, #17614, #19428, #19318, #3578, #7364, #16247, #488, #13932, #20926 ),
 .UNSPECIFIED., .F., .F.,
 ( 4, 2, 2, 2, 2, 2, 2, 2, 2, 2, 2, 2, 2, 2, 2, 2, 2, 2, 2, 4 ),
 ( 0.000000000000000000, 0.0009967370484891052360, 0.001495105572733637905, 0.001993474096978170573, 0.002990211145467237645, 0.003986948193956304717, 0.004983685242445371789, 0.005980422290934439729, 0.006977159339423508536, 0.007973896387912576475, 0.008970633436401644414, 0.009967370484890712354, 0.01046573900913524806, 0.01096410753337978203, 0.01196084458186887425, 0.01295758163035796821, 0.01345595015460251433, 0.01395431867884706391, 0.01495105572733619430, 0.01594779277582532642 ),
 .UNSPECIFIED. ) ;
#422 = PLANE ( 'NONE',  #12245 ) ;
#423 = EDGE_CURVE ( 'NONE', #8239, #10113, #17733, .T. ) ;
#424 = AXIS2_PLACEMENT_3D ( 'NONE', #22195, #15240, #6485 ) ;
#425 = ORIENTED_EDGE ( 'NONE', *, *, #15905, .T. ) ;
#426 = FACE_OUTER_BOUND ( 'NONE', #5369, .T. ) ;
#427 = ORIENTED_EDGE ( 'NONE', *, *, #15678, .F. ) ;
#428 = ORIENTED_EDGE ( 'NONE', *, *, #10191, .F. ) ;
#429 = LINE ( 'NONE', #2033, #16330 ) ;
#430 = CARTESIAN_POINT ( 'NONE',  ( 67.52146002153375548, 70.28876377827108968, -86.83823687282567505 ) ) ;
#431 = CARTESIAN_POINT ( 'NONE',  ( -9.125680706444326162, 185.5535976647744860, 321.2577656795050984 ) ) ;
#432 = CARTESIAN_POINT ( 'NONE',  ( -91.92966151681214626, 79.05204536692272654, 28.63995821788555318 ) ) ;
#433 = DIRECTION ( 'NONE',  ( -0.009138748381789112835, -0.7071067811865462405, -0.7070477234798343558 ) ) ;
#434 = EDGE_LOOP ( 'NONE', ( #5198, #13858 ) ) ;
#435 = CARTESIAN_POINT ( 'NONE',  ( -13.42037733046067238, 183.2664398413913887, 319.4772174752336582 ) ) ;
#436 = AXIS2_PLACEMENT_3D ( 'NONE', #15343, #18765, #6586 ) ;
#437 = ADVANCED_FACE ( 'NONE', ( #9069 ), #20844, .T. ) ;
#438 = FACE_OUTER_BOUND ( 'NONE', #17946, .T. ) ;
#439 = CARTESIAN_POINT ( 'NONE',  ( -15.18250214363469119, 179.4876624324358261, 314.9100870799183554 ) ) ;
#440 = VERTEX_POINT ( 'NONE', #6206 ) ;
#441 = ORIENTED_EDGE ( 'NONE', *, *, #16971, .F. ) ;
#442 = CARTESIAN_POINT ( 'NONE',  ( 2.775557561562891351E-13, 184.8436277385793289, 3.707971429900425164E-14 ) ) ;
#443 = VECTOR ( 'NONE', #5806, 1000.000000000000114 ) ;
#444 = VERTEX_POINT ( 'NONE', #19641 ) ;
#445 = ITEM_DEFINED_TRANSFORMATION ( 'NONE', 'NONE', #12128,  #6292 ) ;
#446 = AXIS2_PLACEMENT_3D ( 'NONE', #5917, #9248, #537 ) ;
#447 = EDGE_LOOP ( 'NONE', ( #11698, #17092 ) ) ;
#448 = AXIS2_PLACEMENT_3D ( 'NONE', #13092, #19825, #9504 ) ;
#449 = AXIS2_PLACEMENT_3D ( 'NONE', #14945, #15170, #16666 ) ;
#450 = DIRECTION ( 'NONE',  ( 0.9999164797902015955, 2.001050586450177755E-22, -0.01292414190464177999 ) ) ;
#451 = EDGE_CURVE ( 'NONE', #8312, #552, #9105, .T. ) ;
#452 = EDGE_CURVE ( 'NONE', #165, #13755, #9315, .T. ) ;
#453 = SPHERICAL_SURFACE ( 'NONE', #18447, 2.000000000000000000 ) ;
#454 = ORIENTED_EDGE ( 'NONE', *, *, #13601, .T. ) ;
#455 = CARTESIAN_POINT ( 'NONE',  ( 3.457270245634820327, 70.35631045439366460, -98.46779458785445627 ) ) ;
#456 = CARTESIAN_POINT ( 'NONE',  ( -9.065023647928146744, 109.7167603697149474, 130.3064260814875013 ) ) ;
#457 = AXIS2_PLACEMENT_3D ( 'NONE', #9188, #1976, #17951 ) ;
#458 = ORIENTED_EDGE ( 'NONE', *, *, #12740, .T. ) ;
#459 = CARTESIAN_POINT ( 'NONE',  ( -41.40281863702377052, 169.1866591894303440, 244.1624146268972595 ) ) ;
#460 = DIRECTION ( 'NONE',  ( 0.000000000000000000, 0.000000000000000000, 1.000000000000000000 ) ) ;
#461 = CARTESIAN_POINT ( 'NONE',  ( 51.64670511766545502, 84.99999999999997158, -27.66980033337678790 ) ) ;
#462 = CARTESIAN_POINT ( 'NONE',  ( 33.37693045445141138, 92.26126280267001789, 80.91304515629593652 ) ) ;
#463 = CARTESIAN_POINT ( 'NONE',  ( 79.99331838321626265, 100.9999999999999858, 4.966068647628683053 ) ) ;
#464 =( BOUNDED_CURVE ( )  B_SPLINE_CURVE ( 3, ( #5130, #22567, #8806, #20870 ),
 .UNSPECIFIED., .F., .T. ) 
 B_SPLINE_CURVE_WITH_KNOTS ( ( 4, 4 ),
 ( 0.4229686233981272414, 0.4841788640348457240 ),
 .UNSPECIFIED. ) 
 CURVE ( )  GEOMETRIC_REPRESENTATION_ITEM ( )  RATIONAL_B_SPLINE_CURVE ( ( 1.000000000000000000, 0.9996877999070342691, 0.9996877999070342691, 1.000000000000000000 ) ) 
 REPRESENTATION_ITEM ( '' )  );
#465 = AXIS2_PLACEMENT_3D ( 'NONE', #19858, #19338, #7694 ) ;
#466 = AXIS2_PLACEMENT_3D ( 'NONE', #6505, #18462, #13187 ) ;
#467 = PRODUCT_RELATED_PRODUCT_CATEGORY ( 'part', '', ( #9543 ) ) ;
#468 = DIRECTION ( 'NONE',  ( -0.000000000000000000, -1.000000000000000000, -0.000000000000000000 ) ) ;
#469 = ORIENTED_EDGE ( 'NONE', *, *, #9836, .T. ) ;
#470 = CARTESIAN_POINT ( 'NONE',  ( 40.93042701181084908, 108.3156947416822362, 71.72688916598494302 ) ) ;
#471 = CARTESIAN_POINT ( 'NONE',  ( -88.41249021357108973, 88.83782181376912490, 50.51791556700484165 ) ) ;
#472 = VECTOR ( 'NONE', #7451, 999.9999999999998863 ) ;
#474 = ORIENTED_EDGE ( 'NONE', *, *, #3932, .F. ) ;
#473 = ORIENTED_EDGE ( 'NONE', *, *, #11263, .F. ) ;
#475 = EDGE_CURVE ( 'NONE', #8008, #17969, #6839, .T. ) ;
#476 = ORIENTED_EDGE ( 'NONE', *, *, #5316, .T. ) ;
#477 = CARTESIAN_POINT ( 'NONE',  ( 1.079165849037564184, 44.99899999999999523, 83.49302606248181746 ) ) ;
#478 = LINE ( 'NONE', #14400, #9234 ) ;
#479 = CIRCLE ( 'NONE', #8172, 10.00000000000001599 ) ;
#480 = CARTESIAN_POINT ( 'NONE',  ( -49.99582398951010731, 170.0000000000000284, 0.6462070952320568828 ) ) ;
#481 = AXIS2_PLACEMENT_3D ( 'NONE', #12195, #19178, #15648 ) ;
#482 = CARTESIAN_POINT ( 'NONE',  ( -91.45377919752192497, 96.73472523270000067, -61.12462174243600543 ) ) ;
#483 = ORIENTED_EDGE ( 'NONE', *, *, #78, .T. ) ;
#484 = LINE ( 'NONE', #12774, #13961 ) ;
#485 = ORIENTED_EDGE ( 'NONE', *, *, #21713, .T. ) ;
#486 = CARTESIAN_POINT ( 'NONE',  ( -164.0000000000000284, 19.17157287525381193, 8.000000000000019540 ) ) ;
#487 = DIRECTION ( 'NONE',  ( -7.125109674403838460E-05, 0.9999848031710253382, -0.005512562950847868688 ) ) ;
#488 = CARTESIAN_POINT ( 'NONE',  ( -79.25692431500161206, 75.13518351147564545, 6.091477897721252255 ) ) ;
#489 = FACE_BOUND ( 'NONE', #18864, .T. ) ;
#490 = DIRECTION ( 'NONE',  ( -0.6916826046072642731, -0.7220860138273257345, 0.01292142092318428193 ) ) ;
#491 = ORIENTED_EDGE ( 'NONE', *, *, #17530, .T. ) ;
#492 = LINE ( 'NONE', #7494, #7808 ) ;
#493 = CARTESIAN_POINT ( 'NONE',  ( -14.05322407132952733, 63.29827626019820741, -14.85614898258057082 ) ) ;
#494 = CARTESIAN_POINT ( 'NONE',  ( 40.97039650227475249, 106.5772003501581082, 92.39653500429078292 ) ) ;
#495 = VERTEX_POINT ( 'NONE', #14623 ) ;
#496 = EDGE_CURVE ( 'NONE', #21893, #14619, #12233, .T. ) ;
#497 = DIRECTION ( 'NONE',  ( -5.440186201345738641E-18, -1.000000000000000000, -1.334940939666364181E-17 ) ) ;
#498 = DIRECTION ( 'NONE',  ( -0.01292394549866743465, -0.005513023399716638837, -0.9999012842304692006 ) ) ;
#499 = ORIENTED_EDGE ( 'NONE', *, *, #15162, .T. ) ;
#500 = AXIS2_PLACEMENT_3D ( 'NONE', #6152, #992, #21857 ) ;
#501 = ORIENTED_EDGE ( 'NONE', *, *, #10667, .T. ) ;
#502 = VECTOR ( 'NONE', #7954, 1000.000000000000114 ) ;
#503 = CARTESIAN_POINT ( 'NONE',  ( -105.3515605809558195, 70.97896074530378030, 31.63944816216639211 ) ) ;
#504 = CARTESIAN_POINT ( 'NONE',  ( 19.56830941617827335, 184.1114337889866874, 316.3329861247396479 ) ) ;
#506 = ORIENTED_EDGE ( 'NONE', *, *, #4777, .T. ) ;
#505 = EDGE_LOOP ( 'NONE', ( #7650, #1698, #13427, #501, #958, #22475 ) ) ;
#507 = CARTESIAN_POINT ( 'NONE',  ( 64.99457118636311748, 105.0000000000000000, -0.8400692238016954638 ) ) ;
#508 = DIRECTION ( 'NONE',  ( -0.9999164797902015955, -6.965998958219364448E-18, 0.01292414190464157182 ) ) ;
#509 = CIRCLE ( 'NONE', #21394, 8.000000000000003553 ) ;
#510 = EDGE_CURVE ( 'NONE', #4157, #19786, #3544, .T. ) ;
#511 = EDGE_CURVE ( 'NONE', #21004, #6936, #16422, .T. ) ;
#512 = CARTESIAN_POINT ( 'NONE',  ( -56.88982296092818558, 126.2575686056375304, 47.57983110662539161 ) ) ;
#513 = LINE ( 'NONE', #7857, #9305 ) ;
#514 = EDGE_CURVE ( 'NONE', #4756, #20909, #13458, .T. ) ;
#515 = ORIENTED_EDGE ( 'NONE', *, *, #10366, .F. ) ;
#516 = LINE ( 'NONE', #744, #20526 ) ;
#517 = CARTESIAN_POINT ( 'NONE',  ( 15.33595178936205627, 187.7751029041553466, 277.1220671345521964 ) ) ;
#518 = CARTESIAN_POINT ( 'NONE',  ( 19.38763582148057907, 184.2660337520671590, 312.0117097956302814 ) ) ;
#519 = VECTOR ( 'NONE', #22182, 1000.000000000000000 ) ;
#520 = CARTESIAN_POINT ( 'NONE',  ( -48.91844876508264406, 94.45452722259994971, 84.00069590936301722 ) ) ;
#521 = CIRCLE ( 'NONE', #1629, 1.999999999999999112 ) ;
#522 = FACE_OUTER_BOUND ( 'NONE', #20407, .T. ) ;
#523 =( NAMED_UNIT ( * ) PLANE_ANGLE_UNIT ( ) SI_UNIT ( $, .RADIAN. ) );
#524 = ADVANCED_FACE ( 'NONE', ( #20667 ), #8478, .T. ) ;
#525 = CARTESIAN_POINT ( 'NONE',  ( 163.9999999999992610, 1.999999999999998224, 53.76161406891480965 ) ) ;
#526 = FACE_OUTER_BOUND ( 'NONE', #19789, .T. ) ;
#527 = EDGE_LOOP ( 'NONE', ( #22645, #19170, #20971, #3651 ) ) ;
#528 = AXIS2_PLACEMENT_3D ( 'NONE', #18973, #11647, #20466 ) ;
#529 = FACE_OUTER_BOUND ( 'NONE', #7929, .T. ) ;
#530 = VERTEX_POINT ( 'NONE', #20541 ) ;
#531 = CARTESIAN_POINT ( 'NONE',  ( -70.91392079944854743, 72.00000000000000000, -84.09052168258642723 ) ) ;
#532 = EDGE_CURVE ( 'NONE', #9660, #4358, #8369, .T. ) ;
#533 = AXIS2_PLACEMENT_3D ( 'NONE', #8570, #17553, #22151 ) ;
#534 = CIRCLE ( 'NONE', #5661, 7.921742784567035400 ) ;
#535 = CARTESIAN_POINT ( 'NONE',  ( -0.4408429396002319645, 70.00000000000001421, -98.97428162928153483 ) ) ;
#536 = FACE_OUTER_BOUND ( 'NONE', #6630, .T. ) ;
#537 = DIRECTION ( 'NONE',  ( -7.125109674243555432E-05, 0.9999848031710253382, -0.005512562950850175003 ) ) ;
#538 = CARTESIAN_POINT ( 'NONE',  ( 4.169604791867612015, 166.7785703876306513, 322.5944574396354483 ) ) ;
#539 = CARTESIAN_POINT ( 'NONE',  ( 79.65664043722195231, 75.20579285942561398, 5.220605708544542978 ) ) ;
#540 = CARTESIAN_POINT ( 'NONE',  ( 161.9999999999998579, 0.000000000000000000, 10.00000000000220091 ) ) ;
#541 = EDGE_CURVE ( 'NONE', #17177, #9516, #1391, .T. ) ;
#542 = ORIENTED_EDGE ( 'NONE', *, *, #423, .F. ) ;
#543 = DIRECTION ( 'NONE',  ( -0.01035335185279156155, -0.005513005182357613894, -0.9999312050732649393 ) ) ;
#544 = CARTESIAN_POINT ( 'NONE',  ( 0.000000000000000000, 0.000000000000000000, 0.000000000000000000 ) ) ;
#545 = AXIS2_PLACEMENT_3D ( 'NONE', #10646, #3288, #5118 ) ;
#546 = DIRECTION ( 'NONE',  ( -7.125109674159588039E-05, 0.9999848031710253382, -0.005512562950848870491 ) ) ;
#547 = ADVANCED_FACE ( 'NONE', ( #15195 ), #4588, .F. ) ;
#548 = CARTESIAN_POINT ( 'NONE',  ( 51.68650743418692173, 107.0878900929417057, 69.97116258175249470 ) ) ;
#549 = LINE ( 'NONE', #12727, #2646 ) ;
#550 = CARTESIAN_POINT ( 'NONE',  ( -90.51365344713411787, 78.00107869518899406, 32.54507930669932847 ) ) ;
#551 = CARTESIAN_POINT ( 'NONE',  ( 79.99331838321626265, 100.9999999999999858, -1.033931352371318058 ) ) ;
#552 = VERTEX_POINT ( 'NONE', #13353 ) ;
#553 = CARTESIAN_POINT ( 'NONE',  ( -15.17867682233058524, 179.5161877312053207, 314.3080855853813205 ) ) ;
#554 = CIRCLE ( 'NONE', #5300, 2.000000000000001332 ) ;
#555 = VERTEX_POINT ( 'NONE', #13234 ) ;
#556 = DIRECTION ( 'NONE',  ( -0.9935244165829104634, -0.1136188085379686713, 0.000000000000000000 ) ) ;
#557 = CARTESIAN_POINT ( 'NONE',  ( -15.13164630670634736, 179.6607342462910708, 313.7313605305386091 ) ) ;
#558 = VERTEX_POINT ( 'NONE', #9880 ) ;
#559 = VERTEX_POINT ( 'NONE', #4926 ) ;
#560 = FACE_OUTER_BOUND ( 'NONE', #1569, .T. ) ;
#561 = EDGE_CURVE ( 'NONE', #10233, #9740, #11615, .T. ) ;
#562 = ORIENTED_EDGE ( 'NONE', *, *, #13386, .T. ) ;
#563 = AXIS2_PLACEMENT_3D ( 'NONE', #12905, #21489, #12783 ) ;
#564 = VERTEX_POINT ( 'NONE', #20430 ) ;
#565 = DIRECTION ( 'NONE',  ( 0.9934404589540163366, 0.1135548637187057675, -0.01346653032742958604 ) ) ;
#566 = ITEM_DEFINED_TRANSFORMATION ( 'NONE', 'NONE', #2585,  #6292 ) ;
#567 = VERTEX_POINT ( 'NONE', #9777 ) ;
#568 = DIRECTION ( 'NONE',  ( -0.1296504907605108559, -0.005475273188901296634, -0.9915446392518419971 ) ) ;
#569 = EDGE_CURVE ( 'NONE', #11631, #5077, #22232, .T. ) ;
#570 = DIRECTION ( 'NONE',  ( -0.01292394549866736179, -0.005513023399721110954, -0.9999012842304692006 ) ) ;
#571 = B_SPLINE_CURVE_WITH_KNOTS ( 'NONE', 3,
 ( #10519, #14093, #4058, #7523, #13059, #2579, #6135, #8528, #22192, #20710, #11994, #22553 ),
 .UNSPECIFIED., .F., .F.,
 ( 4, 2, 2, 2, 2, 4 ),
 ( 0.000000000000000000, 0.0007983727002588449344, 0.001596745400517689869, 0.003193490801035376702, 0.004790236201553063969, 0.006386981602070762078 ),
 .UNSPECIFIED. ) ;
#572 = ORIENTED_EDGE ( 'NONE', *, *, #22537, .F. ) ;
#573 = DIRECTION ( 'NONE',  ( 0.000000000000000000, -1.000000000000000000, 0.000000000000000000 ) ) ;
#574 = ORIENTED_EDGE ( 'NONE', *, *, #16977, .F. ) ;
#575 = DIRECTION ( 'NONE',  ( 0.01292414190464179213, 0.000000000000000000, 0.9999164797902017066 ) ) ;
#576 = CARTESIAN_POINT ( 'NONE',  ( -83.99999999999998579, 37.00000000000000711, 0.000000000000000000 ) ) ;
#577 = DIRECTION ( 'NONE',  ( 0.8585559824929073214, 0.4417096956421488474, -0.2603347262686231400 ) ) ;
#578 = AXIS2_PLACEMENT_3D ( 'NONE', #9864, #20311, #8020 ) ;
#579 = DIRECTION ( 'NONE',  ( -0.1337561903331544455, -0.9909881666746205298, 0.007192708699472569189 ) ) ;
#580 = CARTESIAN_POINT ( 'NONE',  ( 92.43457499998882554, 79.86121811340028387, -31.19724316448930423 ) ) ;
#581 = ORIENTED_EDGE ( 'NONE', *, *, #18788, .F. ) ;
#582 = CARTESIAN_POINT ( 'NONE',  ( -49.99268894125347629, 126.0006686604749291, 0.8887598650694636948 ) ) ;
#583 = CARTESIAN_POINT ( 'NONE',  ( -1.749069042356329984, 81.90747236817705357, -99.14426119037085527 ) ) ;
#584 = EDGE_CURVE ( 'NONE', #17705, #14146, #2869, .T. ) ;
#585 = EDGE_CURVE ( 'NONE', #7846, #1225, #20772, .T. ) ;
#586 = ORIENTED_EDGE ( 'NONE', *, *, #9607, .F. ) ;
#587 = CARTESIAN_POINT ( 'NONE',  ( 42.39538333684826910, 106.8539349815730333, 70.43383574752205334 ) ) ;
#588 = CARTESIAN_POINT ( 'NONE',  ( -88.17180307448359144, 88.85327758763604322, 52.12627907722180254 ) ) ;
#589 =( NAMED_UNIT ( * ) SI_UNIT ( $, .STERADIAN. ) SOLID_ANGLE_UNIT ( ) );
#590 = VECTOR ( 'NONE', #9776, 1000.000000000000114 ) ;
#592 = VERTEX_POINT ( 'NONE', #4683 ) ;
#591 = VERTEX_POINT ( 'NONE', #17124 ) ;
#593 = DIRECTION ( 'NONE',  ( -7.125109674160258889E-05, 0.9999848031710252272, -0.005512562950849897447 ) ) ;
#594 = PLANE ( 'NONE',  #11466 ) ;
#595 = ORIENTED_EDGE ( 'NONE', *, *, #9993, .F. ) ;
#596 = DIRECTION ( 'NONE',  ( -0.01292394549866742424, -0.005513023399720750999, -0.9999012842304693116 ) ) ;
#597 = LINE ( 'NONE', #15896, #8146 ) ;
#598 = DIRECTION ( 'NONE',  ( 0.009760756503428015193, -0.9999378516499566327, 0.005387065077612487526 ) ) ;
#599 = DIRECTION ( 'NONE',  ( -0.9726991065672923042, -0.2316562896908775926, 0.01384960395994898341 ) ) ;
#600 = ORIENTED_EDGE ( 'NONE', *, *, #3820, .F. ) ;
#601 = CARTESIAN_POINT ( 'NONE',  ( 92.13597290369317250, 77.31823782845360427, 29.12178019517720884 ) ) ;
#602 = ORIENTED_EDGE ( 'NONE', *, *, #541, .F. ) ;
#603 = CARTESIAN_POINT ( 'NONE',  ( -55.66434336912175240, 114.2904234907072833, 172.7229050214609174 ) ) ;
#604 = CARTESIAN_POINT ( 'NONE',  ( 49.71850332751439083, 189.5983039071083738, -73.56585792680235159 ) ) ;
#605 = DIRECTION ( 'NONE',  ( 0.000000000000000000, 0.000000000000000000, 1.000000000000000000 ) ) ;
#606 = FACE_OUTER_BOUND ( 'NONE', #18445, .T. ) ;
#607 = DIRECTION ( 'NONE',  ( -0.000000000000000000, -1.000000000000000000, 0.000000000000000000 ) ) ;
#608 = CARTESIAN_POINT ( 'NONE',  ( -40.94748323230124498, 106.8060942374655298, 71.46846058825224191 ) ) ;
#609 = LINE ( 'NONE', #11282, #2017 ) ;
#610 = CARTESIAN_POINT ( 'NONE',  ( -50.62910760614470718, 109.0971227715196363, -45.77181594070039239 ) ) ;
#611 = ORIENTED_EDGE ( 'NONE', *, *, #32, .F. ) ;
#612 = EDGE_CURVE ( 'NONE', #15083, #18866, #14842, .T. ) ;
#613 = FACE_OUTER_BOUND ( 'NONE', #11627, .T. ) ;
#614 = ORIENTED_EDGE ( 'NONE', *, *, #21304, .F. ) ;
#615 = ORIENTED_EDGE ( 'NONE', *, *, #11170, .T. ) ;
#616 = CARTESIAN_POINT ( 'NONE',  ( -84.91224671543740499, 75.00866199770878495, 2.421235374481680136 ) ) ;
#617 =( REPRESENTATION_RELATIONSHIP ('NONE','NONE', #11808, #14914 ) REPRESENTATION_RELATIONSHIP_WITH_TRANSFORMATION ( #16326 )SHAPE_REPRESENTATION_RELATIONSHIP( ) );
#618 = CARTESIAN_POINT ( 'NONE',  ( -88.16310690832857233, 88.22405785602812500, 52.94336900718522543 ) ) ;
#620 = ORIENTED_EDGE ( 'NONE', *, *, #15150, .T. ) ;
#619 = ORIENTED_EDGE ( 'NONE', *, *, #6261, .F. ) ;
#621 = ORIENTED_EDGE ( 'NONE', *, *, #19931, .T. ) ;
#622 = CARTESIAN_POINT ( 'NONE',  ( -38.35540033123504600, 106.2286129618570243, 92.30320912117649357 ) ) ;
#623 = CARTESIAN_POINT ( 'NONE',  ( 41.56623493000984126, 69.99999999999998579, 82.46967996629570052 ) ) ;
#624 = CARTESIAN_POINT ( 'NONE',  ( -41.01898768785987670, 92.04141378167193466, -84.43550307159648582 ) ) ;
#625 = DIRECTION ( 'NONE',  ( 0.01292394549866637994, 0.005513023399719273882, 0.9999012842304692006 ) ) ;
#626 = CARTESIAN_POINT ( 'NONE',  ( 93.23587179807657321, 69.99999999999998579, 30.79757858250317781 ) ) ;
#627 = LINE ( 'NONE', #11303, #11518 ) ;
#628 = CARTESIAN_POINT ( 'NONE',  ( 18.96776859854577069, 184.9744126260587791, 317.4480445392455294 ) ) ;
#629 = CARTESIAN_POINT ( 'NONE',  ( 81.70668847916368804, 104.4142135623730780, -73.64792636435126383 ) ) ;
#630 = DIRECTION ( 'NONE',  ( -0.01292394549866624984, -0.005513023399719273882, -0.9999012842304693116 ) ) ;
#631 =( NAMED_UNIT ( * ) PLANE_ANGLE_UNIT ( ) SI_UNIT ( $, .RADIAN. ) );
#632 = EDGE_CURVE ( 'NONE', #17288, #1407, #18939, .T. ) ;
#633 = DIRECTION ( 'NONE',  ( 0.01035335185279153900, 0.005513005182355262476, 0.9999312050732647172 ) ) ;
#634 = CARTESIAN_POINT ( 'NONE',  ( 49.06020240426833112, 189.6011917897851333, -73.03348424162913943 ) ) ;
#635 = ORIENTED_EDGE ( 'NONE', *, *, #11447, .F. ) ;
#636 = EDGE_LOOP ( 'NONE', ( #1094, #22364, #825, #9647 ) ) ;
#637 = EDGE_CURVE ( 'NONE', #13714, #126, #15945, .T. ) ;
#638 = VERTEX_POINT ( 'NONE', #15306 ) ;
#639 = AXIS2_PLACEMENT_3D ( 'NONE', #5949, #21340, #11248 ) ;
#640 = CARTESIAN_POINT ( 'NONE',  ( 11.98277897518291013, 166.6990352492036891, 81.47011610648978319 ) ) ;
#641 = EDGE_CURVE ( 'NONE', #9573, #8236, #22254, .T. ) ;
#642 = CARTESIAN_POINT ( 'NONE',  ( -12.58664483627419095, 184.6272112293399630, 320.1917372557430213 ) ) ;
#643 = CARTESIAN_POINT ( 'NONE',  ( -54.52327687265813694, 18.00000000000000355, 111.3697098814011781 ) ) ;
#644 = CARTESIAN_POINT ( 'NONE',  ( -88.92875819446121000, 70.43566758519529003, 63.01298426280252585 ) ) ;
#645 = CARTESIAN_POINT ( 'NONE',  ( 49.99582398951007889, 170.0000000000000284, -0.6462070952321007367 ) ) ;
#646 = CARTESIAN_POINT ( 'NONE',  ( 11.77702168924416171, 159.7711821663725971, 324.2021903088674435 ) ) ;
#647 = ADVANCED_FACE ( 'NONE', ( #18837 ), #13561, .F. ) ;
#648 = CARTESIAN_POINT ( 'NONE',  ( -1.163172771417702700, 70.63018678438872655, -89.99248318111824574 ) ) ;
#649 = EDGE_CURVE ( 'NONE', #10347, #7226, #17734, .T. ) ;
#650 = VERTEX_POINT ( 'NONE', #19050 ) ;
#651 = CARTESIAN_POINT ( 'NONE',  ( -10.81485622274934677, 114.1219197046086009, 131.2528221548242584 ) ) ;
#652 = ORIENTED_EDGE ( 'NONE', *, *, #21301, .F. ) ;
#653 = DIRECTION ( 'NONE',  ( 7.855523125929061876E-07, -0.01102495835474593192, -0.9999392232994258611 ) ) ;
#654 = DIRECTION ( 'NONE',  ( 0.000000000000000000, 0.000000000000000000, 1.000000000000000000 ) ) ;
#655 = VECTOR ( 'NONE', #16102, 1000.000000000000000 ) ;
#656 = EDGE_CURVE ( 'NONE', #4221, #1058, #10790, .T. ) ;
#657 = DIRECTION ( 'NONE',  ( 0.9999164797902015955, 2.001050586450178695E-22, -0.01292414190464131335 ) ) ;
#658 = CARTESIAN_POINT ( 'NONE',  ( -8.575531608407624518, 185.9784460181284089, 321.2405749393824976 ) ) ;
#659 = CARTESIAN_POINT ( 'NONE',  ( -90.46145803317399725, 80.27058204906346361, 32.37524683357860056 ) ) ;
#660 = CARTESIAN_POINT ( 'NONE',  ( 0.000000000000000000, 18.00000000000000355, 0.000000000000000000 ) ) ;
#661 = ORIENTED_EDGE ( 'NONE', *, *, #9836, .F. ) ;
#662 = CARTESIAN_POINT ( 'NONE',  ( -14.79896642201964418, 180.4272692235275315, 317.1363243735250421 ) ) ;
#663 = PLANE ( 'NONE',  #13965 ) ;
#664 = CARTESIAN_POINT ( 'NONE',  ( -9.822685604078287724, 184.4798924047493642, 305.4113335104130442 ) ) ;
#665 = VERTEX_POINT ( 'NONE', #6769 ) ;
#666 = EDGE_CURVE ( 'NONE', #5961, #15373, #15750, .T. ) ;
#667 = ORIENTED_EDGE ( 'NONE', *, *, #3510, .T. ) ;
#668 = CARTESIAN_POINT ( 'NONE',  ( -90.40889375659909888, 78.43035437438882695, 33.17122784026039994 ) ) ;
#669 = EDGE_CURVE ( 'NONE', #4632, #17288, #3816, .T. ) ;
#670 = ADVANCED_FACE ( 'NONE', ( #21226 ), #1950, .F. ) ;
#671 = ORIENTED_EDGE ( 'NONE', *, *, #11332, .T. ) ;
#672 = EDGE_CURVE ( 'NONE', #7269, #15892, #7114, .T. ) ;
#673 = AXIS2_PLACEMENT_3D ( 'NONE', #17290, #6819, #13736 ) ;
#674 = CARTESIAN_POINT ( 'NONE',  ( 12.48881921303416398, 189.6164759944761897, 307.6758311242440982 ) ) ;
#675 = ORIENTED_EDGE ( 'NONE', *, *, #17369, .T. ) ;
#676 = EDGE_CURVE ( 'NONE', #9640, #15200, #1828, .T. ) ;
#677 = CARTESIAN_POINT ( 'NONE',  ( -85.63433794141032251, 105.0000000000000000, -69.04172771111927887 ) ) ;
#678 = FACE_OUTER_BOUND ( 'NONE', #20422, .T. ) ;
#679 = CIRCLE ( 'NONE', #12037, 112.5000000000007105 ) ;
#680 = VERTEX_POINT ( 'NONE', #12184 ) ;
#681 = FACE_OUTER_BOUND ( 'NONE', #15154, .T. ) ;
#682 = EDGE_CURVE ( 'NONE', #18467, #17658, #151, .T. ) ;
#683 = FACE_OUTER_BOUND ( 'NONE', #19348, .T. ) ;
#684 = ORIENTED_EDGE ( 'NONE', *, *, #11712, .F. ) ;
#685 = ORIENTED_EDGE ( 'NONE', *, *, #18084, .T. ) ;
#686 = PLANE ( 'NONE',  #15863 ) ;
#687 = LINE ( 'NONE', #9519, #12271 ) ;
#688 = CARTESIAN_POINT ( 'NONE',  ( 157.5176307659770885, 18.00000000000000355, -60.94675664190839370 ) ) ;
#689 = CARTESIAN_POINT ( 'NONE',  ( 35.95309506732430549, 93.50464841319750064, 82.03286182426640494 ) ) ;
#690 = ORIENTED_EDGE ( 'NONE', *, *, #4006, .F. ) ;
#691 = CYLINDRICAL_SURFACE ( 'NONE', #4585, 7.500000000000002665 ) ;
#692 = DIRECTION ( 'NONE',  ( -0.9999164797902015955, -2.001050586450178695E-22, 0.01292414190464131335 ) ) ;
#693 = EDGE_CURVE ( 'NONE', #2734, #11822, #9952, .T. ) ;
#694 = ORIENTED_EDGE ( 'NONE', *, *, #2604, .T. ) ;
#695 = CIRCLE ( 'NONE', #20840, 2.000000000000001332 ) ;
#696 = DIRECTION ( 'NONE',  ( 0.9999164797902017066, 0.000000000000000000, -0.01292414190464174703 ) ) ;
#697 = CARTESIAN_POINT ( 'NONE',  ( -88.29917401736820182, 88.77742970155978242, 50.41907810135165846 ) ) ;
#698 = APPLICATION_PROTOCOL_DEFINITION ( 'draft international standard', 'automotive_design', 1998, #4551 ) ;
#699 = AXIS2_PLACEMENT_3D ( 'NONE', #1518, #3671, #16004 ) ;
#700 = ORIENTED_EDGE ( 'NONE', *, *, #10816, .F. ) ;
#701 = DIRECTION ( 'NONE',  ( -0.01292394549866744159, -0.005513023399721241925, -0.9999012842304693116 ) ) ;
#702 = CARTESIAN_POINT ( 'NONE',  ( -91.00106904273528130, 70.29040131071506892, 61.79648398638329354 ) ) ;
#703 = ORIENTED_EDGE ( 'NONE', *, *, #10621, .T. ) ;
#704 = DIRECTION ( 'NONE',  ( -0.01292394549866738782, -0.005513023399720468239, -0.9999012842304692006 ) ) ;
#705 = DIRECTION ( 'NONE',  ( -7.176269450075762180E-19, 1.000000000000000000, -5.550596000020001457E-17 ) ) ;
#706 = ORIENTED_EDGE ( 'NONE', *, *, #11055, .F. ) ;
#707 = FACE_OUTER_BOUND ( 'NONE', #16939, .T. ) ;
#708 = CARTESIAN_POINT ( 'NONE',  ( 69.24448582912822303, 92.41827837429551096, -85.47053766693686327 ) ) ;
#709 = ORIENTED_EDGE ( 'NONE', *, *, #772, .F. ) ;
#710 = EDGE_CURVE ( 'NONE', #8991, #1318, #19167, .T. ) ;
#711 = DIRECTION ( 'NONE',  ( -0.01292414190464269072, 0.000000000000000000, -0.9999164797902017066 ) ) ;
#712 = EDGE_LOOP ( 'NONE', ( #4652, #19720, #8639 ) ) ;
#713 = CARTESIAN_POINT ( 'NONE',  ( 18.67136755788715519, 169.4339520569534159, -102.9230326054181290 ) ) ;
#714 = CARTESIAN_POINT ( 'NONE',  ( 51.06003536384874053, 189.6011917897851333, -73.05933252543843537 ) ) ;
#715 = DIRECTION ( 'NONE',  ( -0.01292394549866632963, -0.005513023399716958026, -0.9999012842304692006 ) ) ;
#716 = DIRECTION ( 'NONE',  ( -7.125109674025824596E-05, 0.9999848031710253382, -0.005512562950848693549 ) ) ;
#717 = TOROIDAL_SURFACE ( 'NONE', #21293, 4.400000000000000355, 0.4000000000000000222 ) ;
#718 = DIRECTION ( 'NONE',  ( 0.01292394549866738782, 0.005513023399720468239, 0.9999012842304692006 ) ) ;
#719 = VERTEX_POINT ( 'NONE', #21007 ) ;
#720 = CARTESIAN_POINT ( 'NONE',  ( -10.81834107826543168, 163.0306764353018991, 130.9832054571796789 ) ) ;
#721 = DIRECTION ( 'NONE',  ( -0.9999164797902015955, -6.965998958219364448E-18, 0.01292414190464157182 ) ) ;
#722 = FACE_OUTER_BOUND ( 'NONE', #6782, .T. ) ;
#723 = DIRECTION ( 'NONE',  ( 0.9999164797902015955, 2.001050586450178695E-22, -0.01292414190464131335 ) ) ;
#724 = VERTEX_POINT ( 'NONE', #1722 ) ;
#725 = CARTESIAN_POINT ( 'NONE',  ( -10.85567112094788200, 105.6999953372425551, 127.2994028633183348 ) ) ;
#726 = VERTEX_POINT ( 'NONE', #19511 ) ;
#727 = ORIENTED_EDGE ( 'NONE', *, *, #19452, .T. ) ;
#728 = ORIENTED_EDGE ( 'NONE', *, *, #13180, .F. ) ;
#729 = CARTESIAN_POINT ( 'NONE',  ( -85.06887357168608332, 75.00176710950381676, 0.4346775517040236680 ) ) ;
#730 = CARTESIAN_POINT ( 'NONE',  ( 13.58462956591013615, 190.0212252665789094, 307.9296231100185537 ) ) ;
#731 = CIRCLE ( 'NONE', #19768, 4.400000000000000355 ) ;
#732 = ORIENTED_EDGE ( 'NONE', *, *, #9607, .T. ) ;
#733 = ORIENTED_EDGE ( 'NONE', *, *, #1086, .F. ) ;
#734 = MECHANICAL_DESIGN_GEOMETRIC_PRESENTATION_REPRESENTATION (  '', ( #10620 ), #15073 ) ;
#735 = CARTESIAN_POINT ( 'NONE',  ( -38.45083117249132698, 165.6589964890517308, 273.1465725822631612 ) ) ;
#736 = DIRECTION ( 'NONE',  ( 0.01292414190463832269, 0.000000000000000000, 0.9999164797902017066 ) ) ;
#737 = CIRCLE ( 'NONE', #6941, 3.099999999999998757 ) ;
#738 = DIRECTION ( 'NONE',  ( 0.9934404589540163366, 0.1135548637187053511, -0.01346653032743023309 ) ) ;
#739 = DIRECTION ( 'NONE',  ( -0.9999164797902017066, -2.001050586450178931E-22, 0.01292414190464131508 ) ) ;
#740 = CARTESIAN_POINT ( 'NONE',  ( -38.37734285177536009, 94.19957547782772167, -82.31130495469157893 ) ) ;
#741 = CARTESIAN_POINT ( 'NONE',  ( -37.45866066553108453, 94.51302055746239716, 83.85396645971145801 ) ) ;
#742 = EDGE_CURVE ( 'NONE', #12084, #21410, #8941, .T. ) ;
#743 = EDGE_CURVE ( 'NONE', #6677, #18381, #9176, .T. ) ;
#744 = CARTESIAN_POINT ( 'NONE',  ( -146.5000000000000000, 20.00000000000000000, -7.999999999999981348 ) ) ;
#745 = DIRECTION ( 'NONE',  ( 7.125109674160325297E-05, -0.9999848031710252272, 0.005512562950849327591 ) ) ;
#746 = CARTESIAN_POINT ( 'NONE',  ( 19.93997345945722799, 182.7315227521808936, 315.6546791933524787 ) ) ;
#747 = LINE ( 'NONE', #4054, #17299 ) ;
#748 = DIRECTION ( 'NONE',  ( 0.7084451806051504930, 0.7056452299526748684, -0.01304743355500855191 ) ) ;
#749 = SHAPE_REPRESENTATION_RELATIONSHIP ( 'NONE' , 'NONE' ,  #15634, #18406 ) ;
#750 = AXIS2_PLACEMENT_3D ( 'NONE', #20210, #20433, #18609 ) ;
#751 = PRODUCT_DEFINITION_SHAPE ( 'NONE', 'NONE',  #21773 ) ;
#752 = APPLICATION_CONTEXT ( 'automotive_design' ) ;
#753 = CARTESIAN_POINT ( 'NONE',  ( 11.11871845208410825, 165.4774968652965299, 86.48851294219772967 ) ) ;
#754 = DIRECTION ( 'NONE',  ( -0.000000000000000000, -1.000000000000000000, -0.000000000000000000 ) ) ;
#755 = ORIENTED_EDGE ( 'NONE', *, *, #16128, .F. ) ;
#756 = DIRECTION ( 'NONE',  ( 0.8981428216242065554, 0.000000000000000000, 0.4397038457472354223 ) ) ;
#757 = ORIENTED_EDGE ( 'NONE', *, *, #682, .F. ) ;
#758 = ORIENTED_EDGE ( 'NONE', *, *, #13735, .T. ) ;
#759 = DIRECTION ( 'NONE',  ( -0.9999164797902015955, -6.965998958219364448E-18, 0.01292414190464157182 ) ) ;
#760 = CARTESIAN_POINT ( 'NONE',  ( 77.23768650000880598, 75.09868225356437677, -5.328640597094168818 ) ) ;
#761 = DIRECTION ( 'NONE',  ( -0.9999164797902015955, 0.000000000000000000, 0.01292414190464162733 ) ) ;
#762 = CIRCLE ( 'NONE', #16898, 109.9999999999999858 ) ;
#763 = AXIS2_PLACEMENT_3D ( 'NONE', #20757, #10102, #22458 ) ;
#764 = DIRECTION ( 'NONE',  ( 0.01292394549866739996, 0.005513023399721131770, 0.9999012842304692006 ) ) ;
#765 = CONICAL_SURFACE ( 'NONE', #22367, 2.499999999999988010, 1.029744258676651425 ) ;
#766 = ORIENTED_EDGE ( 'NONE', *, *, #125, .T. ) ;
#767 = CARTESIAN_POINT ( 'NONE',  ( -68.86686855361774917, 91.87224768293378929, 85.77506393453893452 ) ) ;
#768 = DIRECTION ( 'NONE',  ( 0.9074876402626336214, 0.002309119226654224137, 0.4200724351096533637 ) ) ;
#769 = CARTESIAN_POINT ( 'NONE',  ( 36.55288090549195346, 94.02752048664900997, -83.45186405039071076 ) ) ;
#770 = PRODUCT_DEFINITION_FORMATION_WITH_SPECIFIED_SOURCE ( 'ANY', '', #21141, .NOT_KNOWN. ) ;
#771 = PLANE ( 'NONE',  #14491 ) ;
#772 = EDGE_CURVE ( 'NONE', #9297, #6510, #5371, .T. ) ;
#773 = DIRECTION ( 'NONE',  ( 7.125109674364536131E-05, -0.9999848031710253382, 0.005512562950849705760 ) ) ;
#774 = CARTESIAN_POINT ( 'NONE',  ( -41.99649215118849810, 170.0000000000000284, 0.5428139599949243221 ) ) ;
#775 = DIRECTION ( 'NONE',  ( 0.000000000000000000, 0.000000000000000000, -1.000000000000000000 ) ) ;
#776 = AXIS2_PLACEMENT_3D ( 'NONE', #10622, #7405, #14094 ) ;
#777 = DIRECTION ( 'NONE',  ( -1.000000000000000000, 0.000000000000000000, 0.000000000000000000 ) ) ;
#778 = EDGE_LOOP ( 'NONE', ( #21060, #476, #15475, #9549 ) ) ;
#779 = CARTESIAN_POINT ( 'NONE',  ( -51.82743751170760049, 114.6914167488026095, 172.2189919798578899 ) ) ;
#780 = ORIENTED_EDGE ( 'NONE', *, *, #380, .T. ) ;
#781 = LINE ( 'NONE', #13421, #11777 ) ;
#782 = CARTESIAN_POINT ( 'NONE',  ( -9.048035673407987645, 185.0480505508585907, 307.9947944869788898 ) ) ;
#783 = ORIENTED_EDGE ( 'NONE', *, *, #14046, .T. ) ;
#784 = VERTEX_POINT ( 'NONE', #16095 ) ;
#785 = AXIS2_PLACEMENT_3D ( 'NONE', #7966, #15001, #20026 ) ;
#786 = CARTESIAN_POINT ( 'NONE',  ( -73.02363241441464936, 95.86457595575431867, 79.19170252361408302 ) ) ;
#787 = ADVANCED_FACE ( 'NONE', ( #15987 ), #20417, .T. ) ;
#788 = CIRCLE ( 'NONE', #20946, 4.999999999999994671 ) ;
#789 = CARTESIAN_POINT ( 'NONE',  ( 53.31522717123864652, 127.4153035195790835, 256.1697555402749913 ) ) ;
#790 = CIRCLE ( 'NONE', #8837, 7.500000000000002665 ) ;
#791 = CARTESIAN_POINT ( 'NONE',  ( 21.11966452740471212, 140.4778767860209143, 86.49708559692255960 ) ) ;
#792 = DIRECTION ( 'NONE',  ( 7.125109674160258889E-05, -0.9999848031710253382, 0.005512562950849898315 ) ) ;
#793 = CARTESIAN_POINT ( 'NONE',  ( 20.96603472858062034, 99.74539563421257071, 74.61103786048234099 ) ) ;
#794 = EDGE_CURVE ( 'NONE', #251, #18403, #137, .T. ) ;
#795 = ORIENTED_EDGE ( 'NONE', *, *, #6607, .F. ) ;
#796 = CARTESIAN_POINT ( 'NONE',  ( 58.06705108255369652, 143.2435277010459060, 43.50008800685101562 ) ) ;
#797 = CIRCLE ( 'NONE', #1538, 11.00000000000000178 ) ;
#798 = EDGE_CURVE ( 'NONE', #12751, #4221, #9395, .T. ) ;
#799 = CARTESIAN_POINT ( 'NONE',  ( -14.20436985759224235, 179.8017517255571818, 320.1469751989672545 ) ) ;
#800 = VERTEX_POINT ( 'NONE', #21662 ) ;
#801 = ORIENTED_EDGE ( 'NONE', *, *, #7186, .T. ) ;
#802 = CARTESIAN_POINT ( 'NONE',  ( -60.48758180977038990, 114.4255654153653552, 169.1364708383153186 ) ) ;
#803 = CARTESIAN_POINT ( 'NONE',  ( -164.0000000000000000, 18.00000000000000355, -53.76161406891256433 ) ) ;
#804 = AXIS2_PLACEMENT_3D ( 'NONE', #2350, #11419, #18214 ) ;
#805 = CYLINDRICAL_SURFACE ( 'NONE', #1413, 4.374999999999991118 ) ;
#806 = CARTESIAN_POINT ( 'NONE',  ( -6.720435043957357024, 86.44819594746830660, 75.42837923485861040 ) ) ;
#807 = ORIENTED_EDGE ( 'NONE', *, *, #20974, .F. ) ;
#808 = DIRECTION ( 'NONE',  ( 0.01292394549866738782, 0.005513023399720468239, 0.9999012842304692006 ) ) ;
#809 = AXIS2_PLACEMENT_3D ( 'NONE', #3079, #12155, #12280 ) ;
#810 = CARTESIAN_POINT ( 'NONE',  ( -8.564669286038160578, 185.5585649246744140, 306.1008109505842754 ) ) ;
#811 = ADVANCED_FACE ( 'NONE', ( #12645 ), #19833, .T. ) ;
#812 = EDGE_LOOP ( 'NONE', ( #5631, #6590, #17195, #4960 ) ) ;
#813 = UNCERTAINTY_MEASURE_WITH_UNIT (LENGTH_MEASURE( 1.000000000000000082E-05 ), #17647, 'distance_accuracy_value', 'NONE');
#814 = VECTOR ( 'NONE', #7229, 1000.000000000000227 ) ;
#815 = SPHERICAL_SURFACE ( 'NONE', #10974, 2.000000000000000000 ) ;
#816 = AXIS2_PLACEMENT_3D ( 'NONE', #13369, #20347, #10018 ) ;
#817 = CARTESIAN_POINT ( 'NONE',  ( -89.31453485712998486, 89.12573045752694156, 51.42325317176502608 ) ) ;
#818 = EDGE_CURVE ( 'NONE', #9599, #7572, #1748, .T. ) ;
#819 = APPLICATION_PROTOCOL_DEFINITION ( 'draft international standard', 'automotive_design', 1998, #14858 ) ;
#820 = AXIS2_PLACEMENT_3D ( 'NONE', #8269, #17121, #15302 ) ;
#821 = B_SPLINE_CURVE_WITH_KNOTS ( 'NONE', 3,
 ( #8550, #15590, #6829, #5090, #12127, #1680 ),
 .UNSPECIFIED., .F., .F.,
 ( 4, 2, 4 ),
 ( 0.002116047826737717588, 0.003573362564032563776, 0.005030677301327409964 ),
 .UNSPECIFIED. ) ;
#822 = VERTEX_POINT ( 'NONE', #9641 ) ;
#823 = CARTESIAN_POINT ( 'NONE',  ( -41.99335710293186708, 126.0006686604749291, 0.7853667298323311341 ) ) ;
#824 = CARTESIAN_POINT ( 'NONE',  ( -52.30302070948153670, 110.0041276461028019, -43.49757385923464170 ) ) ;
#825 = ORIENTED_EDGE ( 'NONE', *, *, #1784, .F. ) ;
#826 = FACE_BOUND ( 'NONE', #21834, .T. ) ;
#827 = AXIS2_PLACEMENT_3D ( 'NONE', #21475, #11159, #4013 ) ;
#828 = FACE_OUTER_BOUND ( 'NONE', #5490, .T. ) ;
#829 = CARTESIAN_POINT ( 'NONE',  ( 1.117803423002105445, 45.00000000000000000, 109.6947150755565161 ) ) ;
#830 = FACE_OUTER_BOUND ( 'NONE', #13990, .T. ) ;
#831 = ORIENTED_EDGE ( 'NONE', *, *, #22112, .T. ) ;
#832 = EDGE_CURVE ( 'NONE', #11858, #8665, #20065, .T. ) ;
#833 = CARTESIAN_POINT ( 'NONE',  ( 33.79255210837673928, 93.51775827232350480, -82.92153020431163668 ) ) ;
#834 = ORIENTED_EDGE ( 'NONE', *, *, #11044, .F. ) ;
#835 = FACE_OUTER_BOUND ( 'NONE', #10421, .T. ) ;
#836 = CARTESIAN_POINT ( 'NONE',  ( -91.27111462898957939, 78.10400798472785766, -30.35002675991158938 ) ) ;
#837 = FACE_OUTER_BOUND ( 'NONE', #2752, .T. ) ;
#838 = CARTESIAN_POINT ( 'NONE',  ( -7.810477471022748475, 165.3506309087785553, 308.2453597648303685 ) ) ;
#839 = VECTOR ( 'NONE', #4920, 999.9999999999998863 ) ;
#840 = CIRCLE ( 'NONE', #8152, 6.000000000000000888 ) ;
#841 = VECTOR ( 'NONE', #4617, 1000.000000000000114 ) ;
#842 = DIRECTION ( 'NONE',  ( -7.125109674403837105E-05, 0.9999848031710252272, -0.005512562950847867821 ) ) ;
#843 = CARTESIAN_POINT ( 'NONE',  ( -64.99457118636308905, 169.9999999999999716, 0.8400692238016759239 ) ) ;
#844 = CARTESIAN_POINT ( 'NONE',  ( 59.65144567478507298, 126.9191314136042479, 166.0817088952479139 ) ) ;
#845 = ORIENTED_EDGE ( 'NONE', *, *, #7582, .F. ) ;
#846 = CARTESIAN_POINT ( 'NONE',  ( 11.80591785795528104, 176.3657631373681056, 324.4430942173937638 ) ) ;
#847 = CIRCLE ( 'NONE', #19145, 2.000000000000004441 ) ;
#848 = VERTEX_POINT ( 'NONE', #12748 ) ;
#849 = EDGE_LOOP ( 'NONE', ( #339, #9089, #22049 ) ) ;
#850 = VERTEX_POINT ( 'NONE', #21454 ) ;
#851 = CARTESIAN_POINT ( 'NONE',  ( -105.3069082217399455, 70.76149960027362340, 31.78775043357526187 ) ) ;
#852 = CARTESIAN_POINT ( 'NONE',  ( -90.15962223546766552, 87.22510259077962758, 51.26146238794839149 ) ) ;
#853 = EDGE_CURVE ( 'NONE', #7530, #5831, #12014, .T. ) ;
#854 = B_SPLINE_CURVE_WITH_KNOTS ( 'NONE', 3,
 ( #18218, #21952, #12942, #4063, #16834, #5778, #2583 ),
 .UNSPECIFIED., .F., .F.,
 ( 4, 3, 4 ),
 ( 0.000000000000000000, 3.076089232684222182E-05, 3.082002332305258858E-05 ),
 .UNSPECIFIED. ) ;
#856 = CARTESIAN_POINT ( 'NONE',  ( 19.46746992363642903, 137.6261247937603969, 113.4190577045456223 ) ) ;
#855 = CIRCLE ( 'NONE', #14444, 3.399999999999986144 ) ;
#858 = VERTEX_POINT ( 'NONE', #2285 ) ;
#857 = ORIENTED_EDGE ( 'NONE', *, *, #10212, .F. ) ;
#859 = AXIS2_PLACEMENT_3D ( 'NONE', #22163, #3207, #9893 ) ;
#860 = CARTESIAN_POINT ( 'NONE',  ( -75.37743570715805674, 94.88086180942337933, 80.20674419475355421 ) ) ;
#861 = DIRECTION ( 'NONE',  ( 0.01292414190464174703, 0.000000000000000000, 0.9999164797902015955 ) ) ;
#862 = CARTESIAN_POINT ( 'NONE',  ( -37.86419661077498944, 93.64690829566940522, -82.87065082828767970 ) ) ;
#863 = CARTESIAN_POINT ( 'NONE',  ( -38.89440990870000547, 93.50952370771440769, 84.88723154575897922 ) ) ;
#864 = EDGE_CURVE ( 'NONE', #9499, #6519, #336, .T. ) ;
#865 = ORIENTED_EDGE ( 'NONE', *, *, #11226, .F. ) ;
#866 = DIRECTION ( 'NONE',  ( 0.9999164797902015955, 2.001050586498092550E-22, -0.01292414190464117457 ) ) ;
#867 = DIRECTION ( 'NONE',  ( -0.8981428216242088869, 0.000000000000000000, 0.4397038457472309814 ) ) ;
#868 = CLOSED_SHELL ( 'NONE', ( #9507, #3329, #670, #6159, #20217, #3581, #16558, #8125, #4845, #18892, #6672, #22153, #20922, #4844, #14910, #4014, #5202, #929, #275, #10956, #17213, #7692, #12682, #11010, #12614, #8148, #7028, #18141, #11464, #12732, #13758, #18689, #18451, #13047, #17407, #9935, #7990, #22077, #9907, #19849, #10891, #1767, #2351, #5694, #9049, #9933, #7246, #15717, #5307, #20059, #20447, #4217, #17804, #17486, #1253, #13446, #10638, #13478 ) ) ;
#869 = CARTESIAN_POINT ( 'NONE',  ( 18.86594229807002421, 185.1130985469481800, 317.5966198224662094 ) ) ;
#870 = PLANE ( 'NONE',  #804 ) ;
#871 = CARTESIAN_POINT ( 'NONE',  ( -3.415012492225389273, 157.2134297314921128, 324.7454257987990331 ) ) ;
#872 = VECTOR ( 'NONE', #6599, 1000.000000000000114 ) ;
#873 = VECTOR ( 'NONE', #11813, 1000.000000000000227 ) ;
#874 = DIRECTION ( 'NONE',  ( 0.000000000000000000, 0.000000000000000000, -1.000000000000000000 ) ) ;
#875 = DIRECTION ( 'NONE',  ( -2.025474946048326158E-22, 1.000000000000000000, -1.876735158486679638E-22 ) ) ;
#876 = ORIENTED_EDGE ( 'NONE', *, *, #13601, .F. ) ;
#877 = DIRECTION ( 'NONE',  ( 0.9999164797902015955, 0.000000000000000000, -0.01292414190463754553 ) ) ;
#878 = EDGE_LOOP ( 'NONE', ( #10525, #21495, #15616, #936 ) ) ;
#879 = CARTESIAN_POINT ( 'NONE',  ( 42.27543525282722214, 106.8832415124691977, 70.46146445762853716 ) ) ;
#880 = EDGE_CURVE ( 'NONE', #13498, #2805, #21780, .T. ) ;
#881 = EDGE_CURVE ( 'NONE', #10347, #20680, #7329, .T. ) ;
#882 = AXIS2_PLACEMENT_3D ( 'NONE', #6049, #14250, #20273 ) ;
#883 = VERTEX_POINT ( 'NONE', #12988 ) ;
#884 = CARTESIAN_POINT ( 'NONE',  ( -50.60913278034716001, 111.9218655255082382, -46.80433714073992491 ) ) ;
#885 = CARTESIAN_POINT ( 'NONE',  ( -40.63089462960165577, 93.08398165842315564, -83.39786430079456636 ) ) ;
#886 = DIRECTION ( 'NONE',  ( -0.01292414190463830014, 0.000000000000000000, -0.9999164797902017066 ) ) ;
#887 = LINE ( 'NONE', #12824, #12247 ) ;
#888 = CARTESIAN_POINT ( 'NONE',  ( -41.94137166082473556, 162.5796238295972671, 273.2086669205137355 ) ) ;
#889 = ORIENTED_EDGE ( 'NONE', *, *, #21935, .T. ) ;
#890 = CARTESIAN_POINT ( 'NONE',  ( 9.882012489055451709, 190.0684914133515235, 274.6858930762247724 ) ) ;
#891 = DIRECTION ( 'NONE',  ( -0.4855951644622631402, -0.0007281815854141815945, 0.8741835081963319487 ) ) ;
#892 = DIRECTION ( 'NONE',  ( -0.9999164797902017066, -6.965998958219367529E-18, 0.01292414190464157182 ) ) ;
#893 = DIRECTION ( 'NONE',  ( -0.000000000000000000, -1.000000000000000000, -0.000000000000000000 ) ) ;
#894 = CARTESIAN_POINT ( 'NONE',  ( 92.43457499998879712, 79.82103140525723006, -31.19724316448930779 ) ) ;
#895 = B_SPLINE_CURVE_WITH_KNOTS ( 'NONE', 3,
 ( #10817, #13911, #20904, #5159, #12201, #19184, #3561, #2076, #9055, #1735 ),
 .UNSPECIFIED., .F., .F.,
 ( 4, 2, 2, 2, 4 ),
 ( -3.258122103462694725E-05, 0.003484391791828337151, 0.007001364804691301812, 0.01051833781755426647, 0.01403531083041723027 ),
 .UNSPECIFIED. ) ;
#896 = DIRECTION ( 'NONE',  ( -7.125109674081160920E-05, 0.9999848031710253382, -0.005512562950849312846 ) ) ;
#897 = CARTESIAN_POINT ( 'NONE',  ( -16.53237339268049055, 177.6255169206013989, 113.6638242950787543 ) ) ;
#898 = AXIS2_PLACEMENT_3D ( 'NONE', #8279, #13568, #18612 ) ;
#899 = VERTEX_POINT ( 'NONE', #14373 ) ;
#900 = CARTESIAN_POINT ( 'NONE',  ( 1.833149449381782370, 126.7813058286111101, 141.8273149490030391 ) ) ;
#901 = ORIENTED_EDGE ( 'NONE', *, *, #13633, .F. ) ;
#902 = CARTESIAN_POINT ( 'NONE',  ( -12.78366430685853672, 181.7268150396907345, 309.3689789245013344 ) ) ;
#903 = ORIENTED_EDGE ( 'NONE', *, *, #7212, .F. ) ;
#904 = VECTOR ( 'NONE', #2432, 1000.000000000000114 ) ;
#905 = ORIENTED_EDGE ( 'NONE', *, *, #14262, .T. ) ;
#906 = AXIS2_PLACEMENT_3D ( 'NONE', #11247, #15610, #15544 ) ;
#907 = FACE_OUTER_BOUND ( 'NONE', #9310, .T. ) ;
#908 = CARTESIAN_POINT ( 'NONE',  ( 11.85847056065619221, 187.7666840159210437, 305.2629551530478125 ) ) ;
#909 = VECTOR ( 'NONE', #4331, 999.9999999999998863 ) ;
#910 = LINE ( 'NONE', #4658, #15177 ) ;
#911 = DIRECTION ( 'NONE',  ( -0.01292394549866740863, -0.005513023399721009472, -0.9999012842304692006 ) ) ;
#912 = VECTOR ( 'NONE', #893, 1000.000000000000000 ) ;
#913 = ORIENTED_EDGE ( 'NONE', *, *, #21546, .T. ) ;
#914 = VECTOR ( 'NONE', #14909, 1000.000000000000114 ) ;
#915 = LINE ( 'NONE', #13745, #2471 ) ;
#916 = CARTESIAN_POINT ( 'NONE',  ( -52.23920841373872292, 126.9191314136037789, 167.5279203743774303 ) ) ;
#917 = ORIENTED_EDGE ( 'NONE', *, *, #10755, .T. ) ;
#918 = DIRECTION ( 'NONE',  ( 0.000000000000000000, -0.000000000000000000, 1.000000000000000000 ) ) ;
#920 = CARTESIAN_POINT ( 'NONE',  ( 64.99457118636310327, 170.0000000000000284, -0.8400692238017243296 ) ) ;
#919 = DIRECTION ( 'NONE',  ( -0.8637520339192008567, -0.002839416958727990648, -0.5039090806998601790 ) ) ;
#921 = DIRECTION ( 'NONE',  ( 0.01292394549866727679, 0.005513023399720742325, 0.9999012842304692006 ) ) ;
#922 = VERTEX_POINT ( 'NONE', #5610 ) ;
#923 =( REPRESENTATION_RELATIONSHIP ('NONE','NONE', #11808, #16508 ) REPRESENTATION_RELATIONSHIP_WITH_TRANSFORMATION ( #18150 )SHAPE_REPRESENTATION_RELATIONSHIP( ) );
#924 = LINE ( 'NONE', #16674, #12690 ) ;
#925 = AXIS2_PLACEMENT_3D ( 'NONE', #14066, #8982, #17618 ) ;
#926 = ADVANCED_FACE ( 'NONE', ( #5825, #16333 ), #3888, .T. ) ;
#927 = CARTESIAN_POINT ( 'NONE',  ( 1.236893267138826732E-14, 0.000000000000000000, 101.0000000000000000 ) ) ;
#928 = ORIENTED_EDGE ( 'NONE', *, *, #6703, .F. ) ;
#929 = ADVANCED_FACE ( 'NONE', ( #681 ), #17534, .F. ) ;
#930 = CARTESIAN_POINT ( 'NONE',  ( 39.75021781620444727, 72.00000000000000000, 86.03367798009509215 ) ) ;
#931 = CARTESIAN_POINT ( 'NONE',  ( -88.18132310388985218, 88.98978577205728868, 51.06603758169391227 ) ) ;
#932 = APPLICATION_PROTOCOL_DEFINITION ( 'draft international standard', 'automotive_design', 1998, #752 ) ;
#933 = ORIENTED_EDGE ( 'NONE', *, *, #14009, .T. ) ;
#934 = DIRECTION ( 'NONE',  ( -0.01292394549866740169, -0.005513023399721021615, -0.9999012842304692006 ) ) ;
#935 = CARTESIAN_POINT ( 'NONE',  ( -51.81471661454150279, 109.8909348587996817, -43.50326120169058441 ) ) ;
#936 = ORIENTED_EDGE ( 'NONE', *, *, #3583, .F. ) ;
#937 = CARTESIAN_POINT ( 'NONE',  ( 79.99331838321626265, 102.0000000000000000, -1.033931352371318058 ) ) ;
#938 = SHAPE_REPRESENTATION ( 'Socket Head Cap Screw L', ( #6292 ), #9601 ) ;
#939 = DIRECTION ( 'NONE',  ( -0.9934404589540161146, -0.1135548637187070442, 0.01346653032743022269 ) ) ;
#940 = ORIENTED_EDGE ( 'NONE', *, *, #6561, .T. ) ;
#941 = AXIS2_PLACEMENT_3D ( 'NONE', #17592, #14035, #11967 ) ;
#942 = FACE_OUTER_BOUND ( 'NONE', #11915, .T. ) ;
#943 = CARTESIAN_POINT ( 'NONE',  ( -91.62437796271720458, 95.71196945526502020, -60.86849236629026905 ) ) ;
#944 = ADVANCED_FACE ( 'NONE', ( #2510 ), #2163, .T. ) ;
#945 = ORIENTED_EDGE ( 'NONE', *, *, #10075, .T. ) ;
#946 = DIRECTION ( 'NONE',  ( -0.9999164797902015955, -6.965998958219364448E-18, 0.01292414190464157182 ) ) ;
#947 = ORIENTED_EDGE ( 'NONE', *, *, #2604, .F. ) ;
#948 = DIRECTION ( 'NONE',  ( 0.9909299940865190504, -0.1338359446631136318, -0.01207007604876911971 ) ) ;
#949 = CARTESIAN_POINT ( 'NONE',  ( 86.44937305384745230, 104.7459436402722446, 68.01917747034273987 ) ) ;
#950 = DIRECTION ( 'NONE',  ( 0.01292394549866733230, 0.005513023399720419666, 0.9999012842304692006 ) ) ;
#951 = CARTESIAN_POINT ( 'NONE',  ( -38.57295527635426424, 106.5467666792623760, 92.13836866384394853 ) ) ;
#952 = EDGE_CURVE ( 'NONE', #10157, #10387, #19843, .T. ) ;
#953 = ORIENTED_EDGE ( 'NONE', *, *, #4737, .T. ) ;
#954 = CARTESIAN_POINT ( 'NONE',  ( 41.56623493000984126, 72.00000000000000000, 82.46967996629570052 ) ) ;
#955 = DIRECTION ( 'NONE',  ( -0.000000000000000000, -1.000000000000000000, 0.000000000000000000 ) ) ;
#956 = VERTEX_POINT ( 'NONE', #16545 ) ;
#957 = CARTESIAN_POINT ( 'NONE',  ( 162.0000000000000000, 1.999999999999998224, -2.262479907570350717E-12 ) ) ;
#958 = ORIENTED_EDGE ( 'NONE', *, *, #16190, .T. ) ;
#959 = VERTEX_POINT ( 'NONE', #18359 ) ;
#960 = ADVANCED_FACE ( 'NONE', ( #15043 ), #20731, .F. ) ;
#961 = DIRECTION ( 'NONE',  ( -0.01292394549866695240, -0.005513023399718316314, -0.9999012842304693116 ) ) ;
#962 = CARTESIAN_POINT ( 'NONE',  ( -90.17329558876596707, 87.04737729605604102, 51.36928819417873626 ) ) ;
#963 = EDGE_CURVE ( 'NONE', #17869, #1319, #1138, .T. ) ;
#964 = EDGE_CURVE ( 'NONE', #2284, #160, #4657, .T. ) ;
#965 = ORIENTED_EDGE ( 'NONE', *, *, #3429, .F. ) ;
#966 = CARTESIAN_POINT ( 'NONE',  ( -154.0000000000000000, 20.00000000000000000, -53.76161406891256433 ) ) ;
#967 = CYLINDRICAL_SURFACE ( 'NONE', #6913, 2.499999999999988010 ) ;
#968 = DIRECTION ( 'NONE',  ( 0.01292394549866733404, 0.005513023399720420534, 0.9999012842304693116 ) ) ;
#969 = CARTESIAN_POINT ( 'NONE',  ( -37.89664629966064524, 96.09134658471360524, 84.97026380959019320 ) ) ;
#970 = ORIENTED_EDGE ( 'NONE', *, *, #22626, .T. ) ;
#971 = CARTESIAN_POINT ( 'NONE',  ( 40.65822637310714782, 72.00000000000000000, 84.25167897319538213 ) ) ;
#972 = CIRCLE ( 'NONE', #7187, 124.0000000000000000 ) ;
#973 = CARTESIAN_POINT ( 'NONE',  ( 24.23788345395560384, 168.9796455556705723, 299.3206640306223676 ) ) ;
#974 = CARTESIAN_POINT ( 'NONE',  ( 17.82481991809018140, 186.4251367409188163, 318.7777147611763553 ) ) ;
#975 = ADVANCED_FACE ( 'NONE', ( #17419 ), #6180, .T. ) ;
#976 = PLANE ( 'NONE',  #10321 ) ;
#977 = DIRECTION ( 'NONE',  ( 0.4397038457472313144, 0.000000000000000000, -0.8981428216242086648 ) ) ;
#978 = ADVANCED_FACE ( 'NONE', ( #5088 ), #11660, .F. ) ;
#979 = VERTEX_POINT ( 'NONE', #20950 ) ;
#980 = CARTESIAN_POINT ( 'NONE',  ( -45.88764766364480607, 166.6314823839715302, 268.8368988230222953 ) ) ;
#981 = DIRECTION ( 'NONE',  ( 0.1136178953597579561, -0.9935164314186356593, 0.004009283626633663132 ) ) ;
#982 = ORIENTED_EDGE ( 'NONE', *, *, #22653, .T. ) ;
#983 = DIRECTION ( 'NONE',  ( 0.9999164797902017066, 0.000000000000000000, -0.01292414190464174703 ) ) ;
#984 = VERTEX_POINT ( 'NONE', #6723 ) ;
#985 = CARTESIAN_POINT ( 'NONE',  ( 41.70036908154883548, 107.1149823552813700, 70.67426363338570638 ) ) ;
#986 = EDGE_CURVE ( 'NONE', #10785, #11013, #915, .T. ) ;
#987 = ORIENTED_EDGE ( 'NONE', *, *, #15352, .T. ) ;
#988 = ORIENTED_EDGE ( 'NONE', *, *, #2448, .F. ) ;
#989 = CARTESIAN_POINT ( 'NONE',  ( 75.19375158121341940, 75.01682528584527176, -2.766602073185969957 ) ) ;
#990 = DIRECTION ( 'NONE',  ( -0.01292394549866737741, -0.005513023399721125699, -0.9999012842304693116 ) ) ;
#991 = DIRECTION ( 'NONE',  ( -0.6979091139780407849, 0.003898296230782323252, 0.7161757269782906832 ) ) ;
#992 = DIRECTION ( 'NONE',  ( -0.01292394549866734098, -0.005513023399720419666, -0.9999012842304692006 ) ) ;
#993 = ORIENTED_EDGE ( 'NONE', *, *, #20376, .T. ) ;
#994 = CARTESIAN_POINT ( 'NONE',  ( 8.732865712828660421, 190.3249964942741883, 274.4707185275763095 ) ) ;
#995 = CARTESIAN_POINT ( 'NONE',  ( 0.000000000000000000, 0.000000000000000000, 0.000000000000000000 ) ) ;
#996 = LINE ( 'NONE', #11330, #11879 ) ;
#997 = CARTESIAN_POINT ( 'NONE',  ( -40.44015661483791035, 106.8832415124692545, 71.53058179755718982 ) ) ;
#998 = CARTESIAN_POINT ( 'NONE',  ( 91.40888322292899204, 77.29711350638434908, -31.45985873596572446 ) ) ;
#999 = ADVANCED_FACE ( 'NONE', ( #4981 ), #4446, .F. ) ;
#1000 = CARTESIAN_POINT ( 'NONE',  ( -10.82440428556346568, 109.7167354332198812, 130.3246429589756872 ) ) ;
#1001 = ADVANCED_FACE ( 'NONE', ( #19114 ), #14443, .F. ) ;
#1002 = DIRECTION ( 'NONE',  ( -7.176269450075762180E-19, 1.000000000000000000, -5.550596000020001457E-17 ) ) ;
#1003 = ORIENTED_EDGE ( 'NONE', *, *, #14860, .T. ) ;
#1004 = CARTESIAN_POINT ( 'NONE',  ( 49.90104868606460542, 189.4888640791102716, -93.42071897647797130 ) ) ;
#1005 = ORIENTED_EDGE ( 'NONE', *, *, #18216, .T. ) ;
#1006 = CARTESIAN_POINT ( 'NONE',  ( -9.128127327470902941, 109.6831586031284758, 124.2118453865659546 ) ) ;
#1007 = CARTESIAN_POINT ( 'NONE',  ( -11.47056600305460350, 183.0990483233374846, 308.4747080909204442 ) ) ;
#1008 = EDGE_LOOP ( 'NONE', ( #15966, #9563, #11679, #21258, #21126, #1572 ) ) ;
#1009 = ORIENTED_EDGE ( 'NONE', *, *, #8835, .T. ) ;
#1010 = CARTESIAN_POINT ( 'NONE',  ( 12.16442896649338223, 187.7168230983759543, 322.9757373289252200 ) ) ;
#1011 = CARTESIAN_POINT ( 'NONE',  ( -46.79684245571608869, 129.3639651298425406, 248.1453739866443868 ) ) ;
#1012 = VECTOR ( 'NONE', #8429, 999.9999999999998863 ) ;
#1013 = CARTESIAN_POINT ( 'NONE',  ( 20.72345578460594595, 149.3062324992208687, 276.4722887938682447 ) ) ;
#1014 = FACE_OUTER_BOUND ( 'NONE', #13248, .T. ) ;
#1015 = ORIENTED_EDGE ( 'NONE', *, *, #13140, .F. ) ;
#1016 = LINE ( 'NONE', #8010, #8056 ) ;
#1017 = EDGE_CURVE ( 'NONE', #1815, #3120, #15233, .T. ) ;
#1018 = VERTEX_POINT ( 'NONE', #4625 ) ;
#1019 = CARTESIAN_POINT ( 'NONE',  ( -106.2880716433168828, 78.18499655656300718, -28.33463432393061154 ) ) ;
#1020 = CARTESIAN_POINT ( 'NONE',  ( 12.21805463999710817, 187.9383611531376914, 322.3984907411651193 ) ) ;
#1021 = LINE ( 'NONE', #20304, #66 ) ;
#1022 = ORIENTED_EDGE ( 'NONE', *, *, #12685, .F. ) ;
#1023 = FACE_BOUND ( 'NONE', #13475, .T. ) ;
#1024 = DIRECTION ( 'NONE',  ( -7.125109674403276030E-05, 0.9999848031710252272, -0.005512562950848280685 ) ) ;
#1025 = DIRECTION ( 'NONE',  ( -1.000000000000000000, -0.000000000000000000, 9.912705577010318154E-17 ) ) ;
#1026 = EDGE_LOOP ( 'NONE', ( #2409, #12741, #5552, #13266 ) ) ;
#1027 = UNCERTAINTY_MEASURE_WITH_UNIT (LENGTH_MEASURE( 1.000000000000000082E-05 ), #12937, 'distance_accuracy_value', 'NONE');
#1028 = FACE_OUTER_BOUND ( 'NONE', #3545, .T. ) ;
#1029 = PRODUCT_DEFINITION ( 'UNKNOWN', '', #9172, #1464 ) ;
#1030 = FACE_OUTER_BOUND ( 'NONE', #15887, .T. ) ;
#1031 = APPLICATION_PROTOCOL_DEFINITION ( 'draft international standard', 'automotive_design', 1998, #19520 ) ;
#1032 = AXIS2_PLACEMENT_3D ( 'NONE', #9960, #10081, #17093 ) ;
#1033 = ORIENTED_EDGE ( 'NONE', *, *, #10803, .F. ) ;
#1034 = FACE_OUTER_BOUND ( 'NONE', #22468, .T. ) ;
#1035 = CARTESIAN_POINT ( 'NONE',  ( -48.90389017660277915, 110.4330569016835852, -43.54387330449551996 ) ) ;
#1036 = EDGE_LOOP ( 'NONE', ( #10873, #8707, #4402, #327 ) ) ;
#1037 = CARTESIAN_POINT ( 'NONE',  ( -5.871648968083819753, 81.34441321561124028, -88.03282711297042340 ) ) ;
#1038 = CARTESIAN_POINT ( 'NONE',  ( -110.8786557059970477, 104.3814432989690602, -67.26907703621752432 ) ) ;
#1039 = ORIENTED_EDGE ( 'NONE', *, *, #20033, .T. ) ;
#1040 = DIRECTION ( 'NONE',  ( 0.9232306267972774094, 0.000000000000000000, -0.3842462878721227826 ) ) ;
#1041 = DIRECTION ( 'NONE',  ( 2.025474946048326158E-22, -1.000000000000000000, 1.876735158486679638E-22 ) ) ;
#1042 = CIRCLE ( 'NONE', #21914, 3.399999999999986144 ) ;
#1044 = DIRECTION ( 'NONE',  ( 0.000000000000000000, 1.000000000000000000, -0.000000000000000000 ) ) ;
#1043 =( REPRESENTATION_RELATIONSHIP ('NONE','NONE', #11808, #2270 ) REPRESENTATION_RELATIONSHIP_WITH_TRANSFORMATION ( #4675 )SHAPE_REPRESENTATION_RELATIONSHIP( ) );
#1045 = EDGE_LOOP ( 'NONE', ( #20981, #3782 ) ) ;
#1046 = CARTESIAN_POINT ( 'NONE',  ( 36.23709397917762942, 94.19957547783377549, -83.27571307199191608 ) ) ;
#1047 = DIRECTION ( 'NONE',  ( 0.000000000000000000, 0.000000000000000000, -1.000000000000000000 ) ) ;
#1048 = ORIENTED_EDGE ( 'NONE', *, *, #2448, .T. ) ;
#1049 = DIRECTION ( 'NONE',  ( 1.387778780781444413E-14, -1.000000000000000000, 0.000000000000000000 ) ) ;
#1050 = DIRECTION ( 'NONE',  ( 0.8981428216242087759, -0.000000000000000000, -0.4397038457472309259 ) ) ;
#1051 = CARTESIAN_POINT ( 'NONE',  ( 1.364374644014609697E-14, 69.99999999999998579, -9.836443712999143722E-15 ) ) ;
#1052 = DIRECTION ( 'NONE',  ( -0.000000000000000000, -1.000000000000000000, -0.000000000000000000 ) ) ;
#1053 = EDGE_CURVE ( 'NONE', #19370, #9718, #14609, .T. ) ;
#1054 = ORIENTED_EDGE ( 'NONE', *, *, #15435, .T. ) ;
#1055 = DIRECTION ( 'NONE',  ( 1.458023040593674599E-16, 0.000000000000000000, 1.000000000000000000 ) ) ;
#1056 = DIRECTION ( 'NONE',  ( 7.125109674160258889E-05, -0.9999848031710252272, 0.005512562950849897447 ) ) ;
#1057 = AXIS2_PLACEMENT_3D ( 'NONE', #17259, #18859, #15329 ) ;
#1058 = VERTEX_POINT ( 'NONE', #22289 ) ;
#1059 = CARTESIAN_POINT ( 'NONE',  ( 48.97873930546568033, 95.44197026330519407, -45.47108626627597516 ) ) ;
#1060 = CARTESIAN_POINT ( 'NONE',  ( -44.86761910970069778, 151.3223208568695952, 257.3069776102678929 ) ) ;
#1061 = VECTOR ( 'NONE', #1259, 1000.000000000000114 ) ;
#1062 = ORIENTED_EDGE ( 'NONE', *, *, #4292, .F. ) ;
#1063 = CARTESIAN_POINT ( 'NONE',  ( 68.31397436809166379, 127.4153035195791119, 255.9758934117053570 ) ) ;
#1064 = EDGE_CURVE ( 'NONE', #15597, #5961, #10038, .T. ) ;
#1065 = CARTESIAN_POINT ( 'NONE',  ( -88.16170457043438091, 88.05983001323437520, 53.05667506944086398 ) ) ;
#1066 =( BOUNDED_CURVE ( )  B_SPLINE_CURVE ( 3, ( #22591, #1958, #12314, #3328 ),
 .UNSPECIFIED., .F., .T. ) 
 B_SPLINE_CURVE_WITH_KNOTS ( ( 4, 4 ),
 ( 5.799006443144740786, 5.860216683781459324 ),
 .UNSPECIFIED. ) 
 CURVE ( )  GEOMETRIC_REPRESENTATION_ITEM ( )  RATIONAL_B_SPLINE_CURVE ( ( 1.000000000000000000, 0.9996877999070342691, 0.9996877999070342691, 1.000000000000000000 ) ) 
 REPRESENTATION_ITEM ( '' )  );
#1067 = CARTESIAN_POINT ( 'NONE',  ( -5.563703806604336499, 326.7005119474492290, 320.3383740725300299 ) ) ;
#1068 = VERTEX_POINT ( 'NONE', #1649 ) ;
#1069 = EDGE_CURVE ( 'NONE', #7401, #8679, #22404, .T. ) ;
#1070 = DIRECTION ( 'NONE',  ( -0.9999164797902015955, -2.001050586450178695E-22, 0.01292414190464131335 ) ) ;
#1071 = CYLINDRICAL_SURFACE ( 'NONE', #2276, 2.000000000000000000 ) ;
#1072 = DIRECTION ( 'NONE',  ( 0.9999164797902015955, 2.045145117964614424E-15, -0.01292414190464167591 ) ) ;
#1073 = FACE_OUTER_BOUND ( 'NONE', #12996, .T. ) ;
#1074 = CIRCLE ( 'NONE', #21586, 2.499999999999988010 ) ;
#1075 = CARTESIAN_POINT ( 'NONE',  ( 79.99331838321640475, 74.99899999999998101, -1.033931352371301404 ) ) ;
#1076 = CARTESIAN_POINT ( 'NONE',  ( -91.41602376139164221, 79.08283919787463390, 28.73514828341261662 ) ) ;
#1077 = CARTESIAN_POINT ( 'NONE',  ( -17.21821209452539847, 315.6014859805258652, 330.9526324688387717 ) ) ;
#1078 = ORIENTED_EDGE ( 'NONE', *, *, #12885, .T. ) ;
#1079 = VECTOR ( 'NONE', #1276, 1000.000000000000000 ) ;
#1080 = ORIENTED_EDGE ( 'NONE', *, *, #1116, .T. ) ;
#1081 = DIRECTION ( 'NONE',  ( 7.125109674403837105E-05, -0.9999848031710252272, 0.005512562950847867821 ) ) ;
#1082 = DIRECTION ( 'NONE',  ( -7.125109674160325297E-05, 0.9999848031710253382, -0.005512562950849328458 ) ) ;
#1083 = CARTESIAN_POINT ( 'NONE',  ( 17.83341159513771856, 184.6399546625437722, 321.1738318148023836 ) ) ;
#1084 = DIRECTION ( 'NONE',  ( 0.000000000000000000, -0.005512562964840580192, -0.9999848057093461140 ) ) ;
#1085 = EDGE_CURVE ( 'NONE', #16346, #2665, #17059, .T. ) ;
#1086 = EDGE_CURVE ( 'NONE', #15798, #10332, #4842, .T. ) ;
#1087 = LINE ( 'NONE', #22190, #15813 ) ;
#1088 = ORIENTED_EDGE ( 'NONE', *, *, #15537, .F. ) ;
#1089 = CARTESIAN_POINT ( 'NONE',  ( 0.000000000000000000, 0.000000000000000000, 0.000000000000000000 ) ) ;
#1090 = CARTESIAN_POINT ( 'NONE',  ( 1.028703311283776507E-14, 45.00000000000000711, 83.99999999999998579 ) ) ;
#1091 = CARTESIAN_POINT ( 'NONE',  ( -63.99205529224568068, 99.43075776215394512, 78.40283286226222970 ) ) ;
#1092 = ORIENTED_EDGE ( 'NONE', *, *, #864, .T. ) ;
#1093 = CARTESIAN_POINT ( 'NONE',  ( -10.86881930386964790, 187.2152970740215494, 276.3440875669132879 ) ) ;
#1094 = ORIENTED_EDGE ( 'NONE', *, *, #6261, .T. ) ;
#1095 = AXIS2_PLACEMENT_3D ( 'NONE', #15139, #6392, #3151 ) ;
#1096 = EDGE_LOOP ( 'NONE', ( #20372, #6109, #189, #21429 ) ) ;
#1097 = MECHANICAL_DESIGN_GEOMETRIC_PRESENTATION_REPRESENTATION (  '', ( #11729 ), #3275 ) ;
#1098 = EDGE_CURVE ( 'NONE', #11124, #4632, #21172, .T. ) ;
#1099 = LINE ( 'NONE', #8092, #15599 ) ;
#1100 = CIRCLE ( 'NONE', #16873, 5.099999999999994316 ) ;
#1101 = EDGE_CURVE ( 'NONE', #13823, #17451, #13826, .T. ) ;
#1102 = ORIENTED_EDGE ( 'NONE', *, *, #1917, .T. ) ;
#1103 = EDGE_CURVE ( 'NONE', #3194, #20616, #20810, .T. ) ;
#1104 = DIRECTION ( 'NONE',  ( 0.8585559824929073214, 0.4417096956421488474, -0.2603347262686231400 ) ) ;
#1105 = CARTESIAN_POINT ( 'NONE',  ( 79.92740525950247843, 75.13699351169599083, -6.133505399301336425 ) ) ;
#1106 = CARTESIAN_POINT ( 'NONE',  ( -20.57109388430227881, 136.7551719540686008, -44.05520973278501629 ) ) ;
#1107 = CARTESIAN_POINT ( 'NONE',  ( -109.5443584724615960, 75.69229587323862063, -10.26624083857044134 ) ) ;
#1108 = DIRECTION ( 'NONE',  ( -0.01292394549866727679, -0.005513023399720743192, -0.9999012842304693116 ) ) ;
#1109 = CARTESIAN_POINT ( 'NONE',  ( 12.82628922073134170, 190.6145596806321407, 307.8497150165550238 ) ) ;
#1110 = DIRECTION ( 'NONE',  ( 7.125109674364534776E-05, -0.9999848031710252272, 0.005512562950849704893 ) ) ;
#1111 = CARTESIAN_POINT ( 'NONE',  ( 42.07978785083213324, 94.68322439548107639, 83.03125727779237764 ) ) ;
#1112 = DIRECTION ( 'NONE',  ( 0.009760756503427994377, -0.9999378516499565217, 0.005387065077612505741 ) ) ;
#1113 = CARTESIAN_POINT ( 'NONE',  ( -52.76977211239809407, 114.4428198097319722, 172.3435807020446191 ) ) ;
#1114 = AXIS2_PLACEMENT_3D ( 'NONE', #8137, #15168, #22120 ) ;
#1115 = AXIS2_PLACEMENT_3D ( 'NONE', #19056, #18843, #4694 ) ;
#1116 = EDGE_CURVE ( 'NONE', #4358, #13904, #17148, .T. ) ;
#1117 = CARTESIAN_POINT ( 'NONE',  ( 92.29888966083395019, 77.12912189587973444, -31.19548940143703675 ) ) ;
#1118 = AXIS2_PLACEMENT_3D ( 'NONE', #18244, #2275, #16321 ) ;
#1119 = DIRECTION ( 'NONE',  ( -5.440186201345738641E-18, -1.000000000000000000, -1.334940939666364181E-17 ) ) ;
#1120 = EDGE_LOOP ( 'NONE', ( #22490, #2558, #19799, #17499, #8659 ) ) ;
#1121 = CARTESIAN_POINT ( 'NONE',  ( 48.91192295135010681, 189.4953846123264611, -92.22510262217610943 ) ) ;
#1122 = ORIENTED_EDGE ( 'NONE', *, *, #20034, .F. ) ;
#1123 = DIRECTION ( 'NONE',  ( 0.9999164797902015955, 0.000000000000000000, -0.01292414190464144692 ) ) ;
#1124 = AXIS2_PLACEMENT_3D ( 'NONE', #11235, #22101, #13312 ) ;
#1125 = CARTESIAN_POINT ( 'NONE',  ( -13.62391555017718048, 183.0616513303022543, 310.0861352889502314 ) ) ;
#1126 = ORIENTED_EDGE ( 'NONE', *, *, #6817, .T. ) ;
#1127 = ORIENTED_EDGE ( 'NONE', *, *, #21240, .T. ) ;
#1128 = CIRCLE ( 'NONE', #3294, 2.000000000000005329 ) ;
#1129 = VECTOR ( 'NONE', #21193, 1000.000000000000114 ) ;
#1130 = DIRECTION ( 'NONE',  ( 0.9999164797902015955, 6.965998958219364448E-18, -0.01292414190464157182 ) ) ;
#1131 = EDGE_CURVE ( 'NONE', #6487, #11658, #18763, .T. ) ;
#1132 = AXIS2_PLACEMENT_3D ( 'NONE', #9374, #4079, #20043 ) ;
#1133 = CARTESIAN_POINT ( 'NONE',  ( 64.99457118636310327, 170.0000000000000284, -0.8400692238017243296 ) ) ;
#1134 = FACE_OUTER_BOUND ( 'NONE', #5167, .T. ) ;
#1135 = VECTOR ( 'NONE', #13086, 999.9999999999998863 ) ;
#1136 = CARTESIAN_POINT ( 'NONE',  ( 58.09936094630035797, 143.2573102595451928, 45.99984121742717491 ) ) ;
#1137 = ORIENTED_EDGE ( 'NONE', *, *, #19027, .T. ) ;
#1138 = LINE ( 'NONE', #13326, #1012 ) ;
#1139 = EDGE_CURVE ( 'NONE', #5652, #18473, #9821, .T. ) ;
#1140 = DIRECTION ( 'NONE',  ( 0.3101392564284315978, 0.9506461370142478273, -0.009250070373107145000 ) ) ;
#1141 = CARTESIAN_POINT ( 'NONE',  ( 38.89810712971356566, 69.99999999999998579, -85.50986645835283184 ) ) ;
#1142 = CARTESIAN_POINT ( 'NONE',  ( 42.33134245603051937, 168.8134312302534283, 56.31375288182659489 ) ) ;
#1143 = CARTESIAN_POINT ( 'NONE',  ( 64.39761729661502443, 113.4706157781613598, -47.02526561348111755 ) ) ;
#1144 = VECTOR ( 'NONE', #20408, 1000.000000000000000 ) ;
#1145 = ORIENTED_EDGE ( 'NONE', *, *, #5482, .T. ) ;
#1146 = LINE ( 'NONE', #22234, #5899 ) ;
#1147 = AXIS2_PLACEMENT_3D ( 'NONE', #3483, #14186, #8983 ) ;
#1148 = FACE_OUTER_BOUND ( 'NONE', #16881, .T. ) ;
#1149 = CARTESIAN_POINT ( 'NONE',  ( -80.05923150692979107, 55.00000000000000000, -4.065642694558677661 ) ) ;
#1150 = VECTOR ( 'NONE', #15189, 1000.000000000000000 ) ;
#1151 = LINE ( 'NONE', #18927, #20877 ) ;
#1152 = CIRCLE ( 'NONE', #424, 3.399999999999985700 ) ;
#1153 = ORIENTED_EDGE ( 'NONE', *, *, #13766, .T. ) ;
#1154 = CARTESIAN_POINT ( 'NONE',  ( -162.0000000000000000, 18.00000000000000355, -53.76161406891256433 ) ) ;
#1155 = FACE_OUTER_BOUND ( 'NONE', #14073, .T. ) ;
#1156 = ADVANCED_FACE ( 'NONE', ( #10257 ), #10710, .T. ) ;
#1157 = ITEM_DEFINED_TRANSFORMATION ( 'NONE', 'NONE', #15133,  #6292 ) ;
#1158 = ADVANCED_FACE ( 'NONE', ( #10937 ), #19649, .T. ) ;
#1160 = ORIENTED_EDGE ( 'NONE', *, *, #8863, .T. ) ;
#1159 = ORIENTED_EDGE ( 'NONE', *, *, #9526, .T. ) ;
#1161 = CIRCLE ( 'NONE', #13994, 112.5000000000007105 ) ;
#1162 = CARTESIAN_POINT ( 'NONE',  ( -52.89202980190114545, 109.4892200475068904, -43.48712180841023667 ) ) ;
#1163 = DIRECTION ( 'NONE',  ( -0.9999164797902015955, -6.965998958219364448E-18, 0.01292414190464157182 ) ) ;
#1164 = DIRECTION ( 'NONE',  ( -0.9934404589540163366, -0.1135548637187060866, 0.01346653032743036840 ) ) ;
#1165 = CARTESIAN_POINT ( 'NONE',  ( 79.99331838321614896, 54.99999999999999289, -1.033931352371314949 ) ) ;
#1166 = EDGE_LOOP ( 'NONE', ( #9714, #12873, #7358 ) ) ;
#1167 = CIRCLE ( 'NONE', #19113, 4.000000000000006217 ) ;
#1168 = CARTESIAN_POINT ( 'NONE',  ( 3.346350515192618058, 81.44153265534507113, -81.07323159506104560 ) ) ;
#1169 = DIRECTION ( 'NONE',  ( -1.000000000000000000, 0.000000000000000000, 0.000000000000000000 ) ) ;
#1170 = DIRECTION ( 'NONE',  ( 0.7070981056135045018, -0.7070960354057282959, -0.005240777737525213927 ) ) ;
#1171 = EDGE_LOOP ( 'NONE', ( #14955, #831, #12321, #20178 ) ) ;
#1172 = CARTESIAN_POINT ( 'NONE',  ( 38.46706438352715196, 91.17157287525387233, -85.27439087629285552 ) ) ;
#1173 = CARTESIAN_POINT ( 'NONE',  ( 1.079165849037564184, 45.00000000000000000, 83.49302606248181746 ) ) ;
#1174 = CIRCLE ( 'NONE', #13648, 1.999999999999998890 ) ;
#1175 = ORIENTED_EDGE ( 'NONE', *, *, #15574, .T. ) ;
#1176 = DIRECTION ( 'NONE',  ( 0.9999164797902015955, 2.001050586450178695E-22, -0.01292414190464131335 ) ) ;
#1177 = CARTESIAN_POINT ( 'NONE',  ( -90.00466877033377955, 70.05991977044968166, 63.23890890537643372 ) ) ;
#1178 = CYLINDRICAL_SURFACE ( 'NONE', #8706, 2.000000000000001332 ) ;
#1179 = FACE_BOUND ( 'NONE', #18318, .T. ) ;
#1180 = DIRECTION ( 'NONE',  ( -1.000000000000000000, 0.000000000000000000, 1.458023040593674599E-16 ) ) ;
#1181 = CARTESIAN_POINT ( 'NONE',  ( 0.000000000000000000, 23.00000000000000000, 0.000000000000000000 ) ) ;
#1182 = VECTOR ( 'NONE', #13570, 999.9999999999998863 ) ;
#1183 = VERTEX_POINT ( 'NONE', #1864 ) ;
#1184 = AXIS2_PLACEMENT_3D ( 'NONE', #9333, #5876, #12914 ) ;
#1185 = DIRECTION ( 'NONE',  ( 0.000000000000000000, 0.000000000000000000, 1.000000000000000000 ) ) ;
#1186 = LINE ( 'NONE', #18732, #11455 ) ;
#1187 = ORIENTED_EDGE ( 'NONE', *, *, #19016, .F. ) ;
#1188 = CIRCLE ( 'NONE', #15492, 0.3999999999999989120 ) ;
#1189 = CARTESIAN_POINT ( 'NONE',  ( -1.614838104868287605, 158.2404303229639595, 324.3837229658399792 ) ) ;
#1190 = CARTESIAN_POINT ( 'NONE',  ( -88.16543564968796431, 88.44947730819713172, 52.74183542837116789 ) ) ;
#1191 = AXIS2_PLACEMENT_3D ( 'NONE', #2311, #2185, #19538 ) ;
#1192 = CARTESIAN_POINT ( 'NONE',  ( 161.9999999999992610, 0.000000000000000000, 53.76161406891478123 ) ) ;
#1194 = ORIENTED_EDGE ( 'NONE', *, *, #21713, .F. ) ;
#1193 = ORIENTED_EDGE ( 'NONE', *, *, #10277, .F. ) ;
#1195 = CARTESIAN_POINT ( 'NONE',  ( -75.01996951961029936, 95.34343679383250958, 80.44883674393967965 ) ) ;
#1196 = FACE_OUTER_BOUND ( 'NONE', #21190, .T. ) ;
#1197 = CARTESIAN_POINT ( 'NONE',  ( -7.151472223503956727, 86.33655068423909995, -75.12481784635232884 ) ) ;
#1198 = CYLINDRICAL_SURFACE ( 'NONE', #14793, 5.100000000000000533 ) ;
#1199 = AXIS2_PLACEMENT_3D ( 'NONE', #18776, #9937, #15135 ) ;
#1200 = CYLINDRICAL_SURFACE ( 'NONE', #8339, 6.250000000000000000 ) ;
#1201 = CARTESIAN_POINT ( 'NONE',  ( -54.77082371508237202, 114.2432787335332307, 171.9760025604842610 ) ) ;
#1202 = AXIS2_PLACEMENT_3D ( 'NONE', #15669, #3891, #6909 ) ;
#1203 = CARTESIAN_POINT ( 'NONE',  ( -52.29989087310946871, 189.4888611505737117, -92.10028044281781945 ) ) ;
#1204 = ORIENTED_EDGE ( 'NONE', *, *, #4008, .F. ) ;
#1205 = ORIENTED_EDGE ( 'NONE', *, *, #10755, .F. ) ;
#1206 = CARTESIAN_POINT ( 'NONE',  ( -16.17007672569239318, 164.4617217281966361, 324.8703238798086659 ) ) ;
#1207 = CARTESIAN_POINT ( 'NONE',  ( 18.69536052806380866, 189.4444907833431273, -101.0667417618365107 ) ) ;
#1208 = CARTESIAN_POINT ( 'NONE',  ( 15.97866707245144902, 185.9292776491716381, 320.3317121505914997 ) ) ;
#1209 = DIRECTION ( 'NONE',  ( 0.9232306267972774094, 0.000000000000000000, -0.3842462878721227826 ) ) ;
#1210 = EDGE_CURVE ( 'NONE', #16785, #22481, #5763, .T. ) ;
#1211 = CARTESIAN_POINT ( 'NONE',  ( -11.21898953668323173, 147.2569162822765350, 277.2143219418639433 ) ) ;
#1212 = VECTOR ( 'NONE', #13349, 999.9999999999998863 ) ;
#1213 = DIRECTION ( 'NONE',  ( -2.664535259100375697E-15, 0.000000000000000000, 1.000000000000000000 ) ) ;
#1214 = CYLINDRICAL_SURFACE ( 'NONE', #18032, 2.000000000000001776 ) ;
#1215 =( BOUNDED_SURFACE ( )  B_SPLINE_SURFACE ( 3, 2, ( 
 ( #2977, #9995, #11265 ),
 ( #22144, #4348, #14957 ),
 ( #13453, #11375, #18275 ),
 ( #2534, #13227, #9535 ),
 ( #18385, #1162, #21908 ),
 ( #17020, #1284, #18707 ),
 ( #14737, #8157, #20323 ),
 ( #21690, #6327, #11610 ),
 ( #5975, #13014, #2653 ),
 ( #19974, #2764, #4243 ),
 ( #16571, #824, #7818 ),
 ( #14853, #6087, #13346 ),
 ( #9663, #935, #4468 ),
 ( #16691, #6200, #11497 ),
 ( #18503, #9772, #1035 ),
 ( #4581, #2864, #10554 ),
 ( #8267, #22248, #13785 ),
 ( #3540, #17576, #15630 ),
 ( #5138, #18831, #12176 ),
 ( #4797, #19043, #15519 ) ),
 .UNSPECIFIED., .F., .F., .T. ) 
 B_SPLINE_SURFACE_WITH_KNOTS ( ( 4, 2, 2, 2, 2, 2, 2, 2, 2, 4 ),
 ( 3, 3 ),
 ( 0.002250506978132263327, 0.003145136895573769423, 0.003592451854294522254, 0.004039766813015275085, 0.004934396730456780747, 0.005829026647898287276, 0.006723656565339793806, 0.007618286482781299468, 0.008512916400222805130, 0.009407546317664310792 ),
 ( 0.000000000000000000, 1.000000000000000000 ),
 .UNSPECIFIED. ) 
 GEOMETRIC_REPRESENTATION_ITEM ( )  RATIONAL_B_SPLINE_SURFACE ( (
 ( 1.000000000000000000, 0.4260362065776441831, 1.000000000000000000),
 ( 1.000000000000000000, 0.4260393075400374374, 1.000000000000000000),
 ( 1.000000000000000000, 0.4294086899200588170, 1.000000000000000000),
 ( 1.000000000000000000, 0.4387845791473878876, 1.000000000000000000),
 ( 1.000000000000000000, 0.4426643443719024407, 1.000000000000000000),
 ( 1.000000000000000000, 0.4514921189388687028, 1.000000000000000000),
 ( 1.000000000000000000, 0.4564487767892564385, 1.000000000000000000),
 ( 1.000000000000000000, 0.4726420716812023137, 1.000000000000000000),
 ( 1.000000000000000000, 0.4853216829651075814, 1.000000000000000000),
 ( 1.000000000000000000, 0.5119006064974717107, 1.000000000000000000),
 ( 1.000000000000000000, 0.5258950471250586345, 1.000000000000000000),
 ( 1.000000000000000000, 0.5546623498312363010, 1.000000000000000000),
 ( 1.000000000000000000, 0.5692926216424040176, 1.000000000000000000),
 ( 1.000000000000000000, 0.5980609968324860359, 1.000000000000000000),
 ( 1.000000000000000000, 0.6123199638066775252, 1.000000000000000000),
 ( 1.000000000000000000, 0.6405585493648041640, 1.000000000000000000),
 ( 1.000000000000000000, 0.6545126017561364584, 1.000000000000000000),
 ( 1.000000000000000000, 0.6813871835234406316, 1.000000000000000000),
 ( 1.000000000000000000, 0.6944185932103925651, 1.000000000000000000),
 ( 1.000000000000000000, 0.7071067811865477948, 1.000000000000000000) ) ) 
 REPRESENTATION_ITEM ( '' )  SURFACE ( )  );
#1216 = DIRECTION ( 'NONE',  ( -0.9934404589540162256, -0.1135548637187057258, 0.01346653032743021748 ) ) ;
#1217 = VERTEX_POINT ( 'NONE', #5644 ) ;
#1219 = CARTESIAN_POINT ( 'NONE',  ( -12.01599076143180511, 185.1584625638569435, 277.0076056079356590 ) ) ;
#1218 = CIRCLE ( 'NONE', #19175, 3.309500000000006992 ) ;
#1220 = ORIENTED_EDGE ( 'NONE', *, *, #9901, .T. ) ;
#1221 = ORIENTED_EDGE ( 'NONE', *, *, #3881, .T. ) ;
#1222 = AXIS2_PLACEMENT_3D ( 'NONE', #4307, #11677, #20277 ) ;
#1223 = EDGE_CURVE ( 'NONE', #14542, #16639, #421, .T. ) ;
#1225 = VERTEX_POINT ( 'NONE', #3689 ) ;
#1224 = ORIENTED_EDGE ( 'NONE', *, *, #8533, .T. ) ;
#1226 = EDGE_CURVE ( 'NONE', #18377, #16716, #5180, .T. ) ;
#1227 = VECTOR ( 'NONE', #114, 1000.000000000000114 ) ;
#1228 = CARTESIAN_POINT ( 'NONE',  ( -50.55759505772823559, 106.8515392057802273, 71.54635382116403264 ) ) ;
#1229 = CARTESIAN_POINT ( 'NONE',  ( -37.16229413748396837, 165.4559312802959994, 269.1306426674853469 ) ) ;
#1230 = CARTESIAN_POINT ( 'NONE',  ( 81.68308784690056257, 75.19231584242493227, 4.986798022879106895 ) ) ;
#1231 = CARTESIAN_POINT ( 'NONE',  ( -48.91807906390275207, 94.48610424851698042, 84.02929899226764121 ) ) ;
#1232 = DIRECTION ( 'NONE',  ( 0.9232306267972777425, 0.000000000000000000, -0.3842462878721221164 ) ) ;
#1233 = ORIENTED_EDGE ( 'NONE', *, *, #7992, .F. ) ;
#1234 = CARTESIAN_POINT ( 'NONE',  ( 5.986268468634207807, 81.99999999999998579, -84.52572088931836447 ) ) ;
#1235 = DIRECTION ( 'NONE',  ( 0.9999164797902015955, 2.044556590511377167E-15, -0.01292414190464178346 ) ) ;
#1236 = TOROIDAL_SURFACE ( 'NONE', #4869, 9.921742784567035400, 2.000000000000000000 ) ;
#1237 = CARTESIAN_POINT ( 'NONE',  ( -41.67747345744867715, 165.9786531560170033, 257.1849355913340673 ) ) ;
#1238 = CIRCLE ( 'NONE', #481, 77.00000000000002842 ) ;
#1239 = EDGE_CURVE ( 'NONE', #13001, #13489, #17742, .T. ) ;
#1240 = DIRECTION ( 'NONE',  ( -2.025474946048326158E-22, 1.000000000000000000, -1.876735158486679638E-22 ) ) ;
#1241 = EDGE_CURVE ( 'NONE', #1225, #14037, #18248, .T. ) ;
#1242 = LINE ( 'NONE', #7987, #18460 ) ;
#1243 = VERTEX_POINT ( 'NONE', #16467 ) ;
#1244 = EDGE_CURVE ( 'NONE', #1880, #592, #5018, .T. ) ;
#1245 = EDGE_LOOP ( 'NONE', ( #20373, #14552, #1137, #6106 ) ) ;
#1246 = CARTESIAN_POINT ( 'NONE',  ( -37.61323352684398458, 61.62499466978435692, 30.16896140480725208 ) ) ;
#1247 = CARTESIAN_POINT ( 'NONE',  ( -9.772617557124883447, 188.0380679982199581, 308.1349344327151130 ) ) ;
#1248 = EDGE_LOOP ( 'NONE', ( #10587, #8874 ) ) ;
#1249 = VECTOR ( 'NONE', #6127, 999.9999999999998863 ) ;
#1250 = CARTESIAN_POINT ( 'NONE',  ( 19.42535155401557390, 139.7551263635816952, -44.58871309782322356 ) ) ;
#1251 = ORIENTED_EDGE ( 'NONE', *, *, #4298, .T. ) ;
#1252 = AXIS2_PLACEMENT_3D ( 'NONE', #51, #5550, #19227 ) ;
#1253 = ADVANCED_FACE ( 'NONE', ( #21809 ), #9052, .F. ) ;
#1254 = AXIS2_PLACEMENT_3D ( 'NONE', #3148, #17173, #10064 ) ;
#1255 = CARTESIAN_POINT ( 'NONE',  ( 14.00406913739424830, 186.9630538133311006, 322.8218460857456193 ) ) ;
#1256 = EDGE_CURVE ( 'NONE', #9573, #164, #19683, .T. ) ;
#1257 = ORIENTED_EDGE ( 'NONE', *, *, #2125, .T. ) ;
#1258 = CARTESIAN_POINT ( 'NONE',  ( -0.3844496095692996329, 327.2789202713466352, 316.8969144942429921 ) ) ;
#1259 = DIRECTION ( 'NONE',  ( 0.9999164797902015955, 4.653667080246435885E-16, -0.01292414190464177999 ) ) ;
#1260 = CARTESIAN_POINT ( 'NONE',  ( 9.196690372329099361, 142.8086146031528187, 274.7267082784171066 ) ) ;
#1261 = LINE ( 'NONE', #15499, #12091 ) ;
#1262 = VECTOR ( 'NONE', #12221, 999.9999999999998863 ) ;
#1263 = DIRECTION ( 'NONE',  ( 3.469446951953611033E-15, 1.000000000000000000, 0.000000000000000000 ) ) ;
#1264 = VERTEX_POINT ( 'NONE', #11052 ) ;
#1265 = CARTESIAN_POINT ( 'NONE',  ( 12.29214828332425924, 188.1889653831995020, 322.0203645085242670 ) ) ;
#1266 = DIRECTION ( 'NONE',  ( 0.9999164797902015955, 6.965998958219364448E-18, -0.01292414190464157182 ) ) ;
#1267 = VECTOR ( 'NONE', #14434, 1000.000000000000114 ) ;
#1268 = ORIENTED_EDGE ( 'NONE', *, *, #21818, .F. ) ;
#1269 = DIRECTION ( 'NONE',  ( 2.449293598294706414E-16, 0.000000000000000000, 1.000000000000000000 ) ) ;
#1270 = VECTOR ( 'NONE', #20131, 1000.000000000000000 ) ;
#1271 = EDGE_CURVE ( 'NONE', #6614, #4445, #16072, .T. ) ;
#1272 = DIRECTION ( 'NONE',  ( -2.025474946048326158E-22, 1.000000000000000000, -1.876735158486679638E-22 ) ) ;
#1273 = CARTESIAN_POINT ( 'NONE',  ( -44.77337549856770238, 180.0561670719389724, 275.2189164286555751 ) ) ;
#1274 = DIRECTION ( 'NONE',  ( 2.025474946048326158E-22, -1.000000000000000000, 1.876735158486679638E-22 ) ) ;
#1275 = AXIS2_PLACEMENT_3D ( 'NONE', #8915, #6967, #5234 ) ;
#1276 = DIRECTION ( 'NONE',  ( -1.396592535537253658E-14, 0.000000000000000000, -1.000000000000000000 ) ) ;
#1277 = CARTESIAN_POINT ( 'NONE',  ( -10.85567112094788200, 105.6999953372425409, 127.2994028633183063 ) ) ;
#1278 = EDGE_CURVE ( 'NONE', #7668, #3399, #21703, .T. ) ;
#1279 = PRODUCT_CONTEXT ( 'NONE', #19520, 'mechanical' ) ;
#1280 = AXIS2_PLACEMENT_3D ( 'NONE', #1801, #20431, #6334 ) ;
#1282 = ORIENTED_EDGE ( 'NONE', *, *, #11887, .F. ) ;
#1281 = ORIENTED_EDGE ( 'NONE', *, *, #11747, .T. ) ;
#1283 = CIRCLE ( 'NONE', #19225, 1.999999999999997780 ) ;
#1284 = CARTESIAN_POINT ( 'NONE',  ( -52.89610439416505727, 109.5992314273289026, -43.48767569858423343 ) ) ;
#1285 = LINE ( 'NONE', #4679, #5607 ) ;
#1286 = CARTESIAN_POINT ( 'NONE',  ( 54.52327687265659506, 20.00000000000000000, -111.3697098814019455 ) ) ;
#1287 = LINE ( 'NONE', #22357, #13681 ) ;
#1288 = VERTEX_POINT ( 'NONE', #2323 ) ;
#1289 = CARTESIAN_POINT ( 'NONE',  ( 41.20572975695933593, 107.5148010522800064, 93.02654324256212703 ) ) ;
#1290 = CARTESIAN_POINT ( 'NONE',  ( 65.76886434875187604, 106.9149828242082947, 59.06553216729307110 ) ) ;
#1291 = VERTEX_POINT ( 'NONE', #5748 ) ;
#1292 = CARTESIAN_POINT ( 'NONE',  ( 33.82085273160093664, 93.50464841319750064, -82.93470554904388337 ) ) ;
#1293 = EDGE_LOOP ( 'NONE', ( #8266, #22233 ) ) ;
#1294 = DIRECTION ( 'NONE',  ( -0.01292414190464022741, 0.000000000000000000, -0.9999164797902017066 ) ) ;
#1295 = FACE_OUTER_BOUND ( 'NONE', #10911, .T. ) ;
#1296 = CIRCLE ( 'NONE', #3486, 120.0000000000000000 ) ;
#1297 = CARTESIAN_POINT ( 'NONE',  ( 106.1909711380429542, 71.47214965576931434, 28.69631340039671841 ) ) ;
#1298 = CARTESIAN_POINT ( 'NONE',  ( 48.31072223536619958, 166.8507685304810764, 256.0170097695137201 ) ) ;
#1299 = ADVANCED_FACE ( 'NONE', ( #19872 ), #18518, .F. ) ;
#1300 = CARTESIAN_POINT ( 'NONE',  ( 1.833149449381782370, 126.7813058286111101, 141.8273149490030391 ) ) ;
#1301 = EDGE_CURVE ( 'NONE', #17005, #20235, #11278, .T. ) ;
#1302 = VERTEX_POINT ( 'NONE', #9675 ) ;
#1303 = CIRCLE ( 'NONE', #11193, 2.000000000000001332 ) ;
#1304 = CARTESIAN_POINT ( 'NONE',  ( -66.44851505496320954, 169.3797848675314128, -111.6488252521261160 ) ) ;
#1305 = CARTESIAN_POINT ( 'NONE',  ( -44.65183966190961939, 161.1467762486291520, 27.22731394492822687 ) ) ;
#1306 = EDGE_LOOP ( 'NONE', ( #12089, #16174 ) ) ;
#1307 = CARTESIAN_POINT ( 'NONE',  ( 41.19638261157623305, 121.2962013336460814, 247.0525242307099347 ) ) ;
#1308 = CARTESIAN_POINT ( 'NONE',  ( -89.99197688737933731, 88.74347365508511132, 52.47095576274720941 ) ) ;
#1309 = STYLED_ITEM ( 'NONE', ( #15085 ), #9845 ) ;
#1310 = ORIENTED_EDGE ( 'NONE', *, *, #20423, .T. ) ;
#1311 = CARTESIAN_POINT ( 'NONE',  ( 58.90831880861169623, 126.6021325681202825, 108.5873850519959092 ) ) ;
#1312 = DIRECTION ( 'NONE',  ( -0.01292394549866632963, -0.005513023399716958026, -0.9999012842304692006 ) ) ;
#1313 = DIRECTION ( 'NONE',  ( -0.01292394549866739822, -0.005513023399721269681, -0.9999012842304692006 ) ) ;
#1314 = CARTESIAN_POINT ( 'NONE',  ( -44.26142469380095434, 168.8134312302532862, 57.43298357076854899 ) ) ;
#1315 = CARTESIAN_POINT ( 'NONE',  ( -89.22767861003021039, 80.31838830481383695, -30.18953644180660234 ) ) ;
#1316 = DIRECTION ( 'NONE',  ( -0.01257542709085761497, -0.04040699277118586091, -0.9991041655246323261 ) ) ;
#1317 = CARTESIAN_POINT ( 'NONE',  ( -51.24077369867691800, 189.4960777121730473, -90.80487779002250193 ) ) ;
#1318 = VERTEX_POINT ( 'NONE', #2778 ) ;
#1319 = VERTEX_POINT ( 'NONE', #12900 ) ;
#1320 = DIRECTION ( 'NONE',  ( -0.01292394549866632963, -0.005513023399716958026, -0.9999012842304692006 ) ) ;
#1321 = DIRECTION ( 'NONE',  ( 0.9999164797902017066, 0.000000000000000000, -0.01292414190463751951 ) ) ;
#1322 = DIRECTION ( 'NONE',  ( 7.125109674403837105E-05, -0.9999848031710252272, 0.005512562950847867821 ) ) ;
#1323 = CARTESIAN_POINT ( 'NONE',  ( -59.95575053096360563, 114.2084250825692209, 165.7205294013835157 ) ) ;
#1324 = CARTESIAN_POINT ( 'NONE',  ( -8.866921938745853993, 144.9029155259317179, 276.3123546325696225 ) ) ;
#1325 = VERTEX_POINT ( 'NONE', #16703 ) ;
#1326 = DIRECTION ( 'NONE',  ( -0.9232306267972777425, 0.000000000000000000, 0.3842462878721220054 ) ) ;
#1327 = AXIS2_PLACEMENT_3D ( 'NONE', #18507, #7930, #13351 ) ;
#1328 = CARTESIAN_POINT ( 'NONE',  ( 44.03004128744986190, 171.4878726268958360, -75.33468125154308836 ) ) ;
#1329 = EDGE_LOOP ( 'NONE', ( #16290, #11373, #17539, #13804, #17308 ) ) ;
#1330 = CARTESIAN_POINT ( 'NONE',  ( -10.69950344851409163, 186.1885126486754700, 276.9478893194735747 ) ) ;
#1331 = VERTEX_POINT ( 'NONE', #16367 ) ;
#1332 = CARTESIAN_POINT ( 'NONE',  ( -64.34562386414329183, 87.00751446224754204, 51.04789940634336887 ) ) ;
#1334 = ORIENTED_EDGE ( 'NONE', *, *, #18596, .F. ) ;
#1333 = VERTEX_POINT ( 'NONE', #18288 ) ;
#1335 = CARTESIAN_POINT ( 'NONE',  ( 48.02316444802085016, 166.7281037598372961, 233.7692061953857774 ) ) ;
#1336 = DIRECTION ( 'NONE',  ( 3.552713678800500929E-15, 0.000000000000000000, 1.000000000000000000 ) ) ;
#1337 = AXIS2_PLACEMENT_3D ( 'NONE', #19395, #892, #13182 ) ;
#1338 = CARTESIAN_POINT ( 'NONE',  ( -106.8724933792760652, 79.04398536104956463, -26.04362031086678897 ) ) ;
#1339 = DIRECTION ( 'NONE',  ( 1.000000000000000000, 0.000000000000000000, 1.372099599554301422E-14 ) ) ;
#1340 = CARTESIAN_POINT ( 'NONE',  ( 20.72467744229798825, 186.0120790718647754, 276.2495570520306387 ) ) ;
#1341 = ORIENTED_EDGE ( 'NONE', *, *, #10232, .F. ) ;
#1342 = DIRECTION ( 'NONE',  ( 7.125109674403277385E-05, -0.9999848031710253382, 0.005512562950848281552 ) ) ;
#1343 = CARTESIAN_POINT ( 'NONE',  ( 7.055447609860086011, 81.90747236817705357, -85.92399523110739779 ) ) ;
#1344 = DIRECTION ( 'NONE',  ( -0.000000000000000000, -1.000000000000000000, -0.000000000000000000 ) ) ;
#1345 = PLANE ( 'NONE',  #174 ) ;
#1346 = EDGE_CURVE ( 'NONE', #680, #1692, #13503, .T. ) ;
#1347 = CARTESIAN_POINT ( 'NONE',  ( 88.62677304471942819, 79.89796367043616954, -31.25921585370831224 ) ) ;
#1348 = DIRECTION ( 'NONE',  ( 0.000000000000000000, 0.000000000000000000, -1.000000000000000000 ) ) ;
#1349 = EDGE_CURVE ( 'NONE', #15641, #4119, #16444, .T. ) ;
#1350 = ORIENTED_EDGE ( 'NONE', *, *, #13991, .F. ) ;
#1351 = CARTESIAN_POINT ( 'NONE',  ( 1.364374644014609697E-14, 69.99999999999998579, -9.836443712999143722E-15 ) ) ;
#1352 = CARTESIAN_POINT ( 'NONE',  ( -10.17049351323417561, 187.7283718258219949, 308.1773159039984762 ) ) ;
#1353 = ORIENTED_EDGE ( 'NONE', *, *, #7238, .T. ) ;
#1354 = CARTESIAN_POINT ( 'NONE',  ( 5.986268468634207807, 69.99999999999998579, -84.52572088931836447 ) ) ;
#1355 = EDGE_LOOP ( 'NONE', ( #16218, #8476, #413, #7161 ) ) ;
#1356 =( REPRESENTATION_RELATIONSHIP ('NONE','NONE', #11808, #938 ) REPRESENTATION_RELATIONSHIP_WITH_TRANSFORMATION ( #19155 )SHAPE_REPRESENTATION_RELATIONSHIP( ) );
#1357 = CARTESIAN_POINT ( 'NONE',  ( 16.40873467035000033, 185.6567299720572635, 322.3321779654820602 ) ) ;
#1358 = EDGE_CURVE ( 'NONE', #6866, #8785, #22263, .T. ) ;
#1359 = ADVANCED_FACE ( 'NONE', ( #837 ), #7833, .T. ) ;
#1360 = CARTESIAN_POINT ( 'NONE',  ( 45.44350069997184249, 168.6907664596096765, 34.02200722522287180 ) ) ;
#1361 = FACE_OUTER_BOUND ( 'NONE', #2181, .T. ) ;
#1362 = CARTESIAN_POINT ( 'NONE',  ( 18.01056092802276964, 145.8310346079609872, 276.1989901147027240 ) ) ;
#1363 = EDGE_CURVE ( 'NONE', #134, #18610, #14624, .T. ) ;
#1364 = CARTESIAN_POINT ( 'NONE',  ( 13.70891000273312343, 189.9149113544312399, 320.7681615485908537 ) ) ;
#1365 = VERTEX_POINT ( 'NONE', #13243 ) ;
#1366 = DIRECTION ( 'NONE',  ( -0.01292414190464132896, 0.000000000000000000, -0.9999164797902015955 ) ) ;
#1367 = DIRECTION ( 'NONE',  ( 1.000000000000000000, -0.000000000000000000, -1.458023040593674599E-16 ) ) ;
#1368 = FACE_OUTER_BOUND ( 'NONE', #21089, .T. ) ;
#1369 = ORIENTED_EDGE ( 'NONE', *, *, #4719, .F. ) ;
#1370 = EDGE_CURVE ( 'NONE', #19478, #5262, #3205, .T. ) ;
#1371 = DIRECTION ( 'NONE',  ( 0.01292394549866733404, 0.005513023399720420534, 0.9999012842304693116 ) ) ;
#1372 = EDGE_CURVE ( 'NONE', #16531, #4876, #8378, .T. ) ;
#1373 = VERTEX_POINT ( 'NONE', #6775 ) ;
#1374 = CARTESIAN_POINT ( 'NONE',  ( -16.19592461668972661, 164.4506956813972067, 322.8705213113477726 ) ) ;
#1375 = DIRECTION ( 'NONE',  ( -0.000000000000000000, -1.000000000000000000, 0.000000000000000000 ) ) ;
#1376 = CARTESIAN_POINT ( 'NONE',  ( -12.01575389182678499, 182.4076787623492066, 322.7174846376903474 ) ) ;
#1377 = EDGE_CURVE ( 'NONE', #22319, #11631, #22483, .T. ) ;
#1378 = CARTESIAN_POINT ( 'NONE',  ( -25.68841619517593955, 324.3516952872404318, 308.6004965912300690 ) ) ;
#1379 = LINE ( 'NONE', #8465, #21418 ) ;
#1380 = CARTESIAN_POINT ( 'NONE',  ( 54.52327687265660927, 20.00000000000000000, 111.3697098814019029 ) ) ;
#1381 = AXIS2_PLACEMENT_3D ( 'NONE', #18157, #9162, #7454 ) ;
#1382 = DIRECTION ( 'NONE',  ( 0.01292394549866733230, 0.005513023399720419666, 0.9999012842304692006 ) ) ;
#1383 = EDGE_CURVE ( 'NONE', #3455, #12065, #5163, .T. ) ;
#1384 = PRODUCT_CONTEXT ( 'NONE', #22565, 'mechanical' ) ;
#1385 = EDGE_LOOP ( 'NONE', ( #12013, #19855, #11519, #22409, #1884 ) ) ;
#1386 = CARTESIAN_POINT ( 'NONE',  ( 52.34460878051607580, 78.91761970611439381, 26.32568957529414178 ) ) ;
#1387 = EDGE_CURVE ( 'NONE', #16056, #3377, #16085, .T. ) ;
#1388 = ORIENTED_EDGE ( 'NONE', *, *, #17750, .F. ) ;
#1389 = CARTESIAN_POINT ( 'NONE',  ( -164.0000000000000000, 18.00000000000000355, 0.000000000000000000 ) ) ;
#1390 = DIRECTION ( 'NONE',  ( -0.01292414190464218071, -1.902755938799532120E-22, -0.9999164797902017066 ) ) ;
#1391 = LINE ( 'NONE', #11847, #17880 ) ;
#1392 = ORIENTED_EDGE ( 'NONE', *, *, #10556, .F. ) ;
#1393 = CARTESIAN_POINT ( 'NONE',  ( 51.76881283800809541, 109.6007514900105093, -44.84050130987714056 ) ) ;
#1394 = VERTEX_POINT ( 'NONE', #8043 ) ;
#1395 = DIRECTION ( 'NONE',  ( 1.000000000000000000, 0.000000000000000000, 0.000000000000000000 ) ) ;
#1396 = LINE ( 'NONE', #6454, #3814 ) ;
#1397 = DIRECTION ( 'NONE',  ( -0.9999164797902015955, 0.000000000000000000, 0.01292414190464162733 ) ) ;
#1398 = DIRECTION ( 'NONE',  ( 0.000000000000000000, 0.000000000000000000, -1.000000000000000000 ) ) ;
#1399 = AXIS2_PLACEMENT_3D ( 'NONE', #7003, #12191, #342 ) ;
#1400 = EDGE_CURVE ( 'NONE', #8332, #15977, #20338, .T. ) ;
#1401 = ORIENTED_EDGE ( 'NONE', *, *, #1478, .F. ) ;
#1402 = CARTESIAN_POINT ( 'NONE',  ( -10.81199549121517123, 73.97252985729198826, 131.4741515573008712 ) ) ;
#1403 = AXIS2_PLACEMENT_3D ( 'NONE', #9251, #7191, #14220 ) ;
#1404 = ORIENTED_EDGE ( 'NONE', *, *, #20725, .T. ) ;
#1405 = CARTESIAN_POINT ( 'NONE',  ( 49.40325090546203057, 96.06183802811887062, -46.49246881160556910 ) ) ;
#1406 = DIRECTION ( 'NONE',  ( -0.01292394549866736873, -0.005513023399721228915, -0.9999012842304690896 ) ) ;
#1407 = VERTEX_POINT ( 'NONE', #22369 ) ;
#1408 = CONICAL_SURFACE ( 'NONE', #5410, 2.499999999999988010, 1.029744258676651425 ) ;
#1409 = DIRECTION ( 'NONE',  ( -0.1296504907605101897, -0.005475273188901850878, -0.9915446392518421082 ) ) ;
#1410 = CARTESIAN_POINT ( 'NONE',  ( -90.10913265094163194, 87.45414967491383607, 51.12188757306625320 ) ) ;
#1412 = ORIENTED_EDGE ( 'NONE', *, *, #22523, .T. ) ;
#1411 = ORIENTED_EDGE ( 'NONE', *, *, #19388, .F. ) ;
#1413 = AXIS2_PLACEMENT_3D ( 'NONE', #12754, #19723, #2413 ) ;
#1414 = EDGE_CURVE ( 'NONE', #3247, #10313, #19707, .T. ) ;
#1415 = CARTESIAN_POINT ( 'NONE',  ( -73.83063990018285949, 96.00169183596570122, 81.54214722377805913 ) ) ;
#1416 = DIRECTION ( 'NONE',  ( -0.01292394549866733230, -0.005513023399720419666, -0.9999012842304692006 ) ) ;
#1417 = CARTESIAN_POINT ( 'NONE',  ( 42.77078531357724245, 106.9149828242082947, 59.36278743109983225 ) ) ;
#1418 = ORIENTED_EDGE ( 'NONE', *, *, #21040, .T. ) ;
#1419 = CARTESIAN_POINT ( 'NONE',  ( -88.17578298076553267, 88.98131632899244892, 51.70423481999122828 ) ) ;
#1420 = CARTESIAN_POINT ( 'NONE',  ( 44.31808358225305966, 164.8106407359766763, -53.04939224934937414 ) ) ;
#1421 = CARTESIAN_POINT ( 'NONE',  ( -51.17105351027176141, 189.4989811950858609, -90.27908403945292548 ) ) ;
#1422 = ORIENTED_EDGE ( 'NONE', *, *, #641, .T. ) ;
#1423 = VERTEX_POINT ( 'NONE', #11622 ) ;
#1424 = ORIENTED_EDGE ( 'NONE', *, *, #12432, .F. ) ;
#1425 = CARTESIAN_POINT ( 'NONE',  ( -64.03197570747913403, 99.62212517233105302, 75.31426563926737572 ) ) ;
#1426 = CARTESIAN_POINT ( 'NONE',  ( -88.18368518054532501, 87.00751446224754204, 51.35601162712541168 ) ) ;
#1427 = CARTESIAN_POINT ( 'NONE',  ( 90.66698955146013361, 79.16774870435551748, -29.00429242512963768 ) ) ;
#1428 = DIRECTION ( 'NONE',  ( 0.01292394549866738782, 0.005513023399720468239, 0.9999012842304692006 ) ) ;
#1429 = AXIS2_PLACEMENT_3D ( 'NONE', #11749, #10141, #6471 ) ;
#1430 = CARTESIAN_POINT ( 'NONE',  ( -2.684107246038483385, 142.9527971194642078, 275.3366952467220017 ) ) ;
#1431 = EDGE_CURVE ( 'NONE', #1288, #17029, #10349, .T. ) ;
#1432 = EDGE_LOOP ( 'NONE', ( #10019, #11509, #17070, #14854 ) ) ;
#1433 = CARTESIAN_POINT ( 'NONE',  ( 0.000000000000000000, 0.000000000000000000, 0.000000000000000000 ) ) ;
#1434 = CARTESIAN_POINT ( 'NONE',  ( -56.11438623100815448, 126.5883500096207683, 107.5739081604535414 ) ) ;
#1435 = CARTESIAN_POINT ( 'NONE',  ( 41.42451162475439475, 125.7553391191873544, -44.79586833841344173 ) ) ;
#1436 = ORIENTED_EDGE ( 'NONE', *, *, #18757, .T. ) ;
#1437 = ORIENTED_EDGE ( 'NONE', *, *, #8759, .T. ) ;
#1438 = DIRECTION ( 'NONE',  ( 0.01292394549866731843, 0.005513023399720594006, 0.9999012842304693116 ) ) ;
#1439 = CIRCLE ( 'NONE', #6192, 78.99999999999998579 ) ;
#1440 = ORIENTED_EDGE ( 'NONE', *, *, #17648, .T. ) ;
#1441 = EDGE_CURVE ( 'NONE', #21136, #10347, #7244, .T. ) ;
#1442 = FACE_OUTER_BOUND ( 'NONE', #4234, .T. ) ;
#1443 = DIRECTION ( 'NONE',  ( -0.000000000000000000, -1.000000000000000000, 0.000000000000000000 ) ) ;
#1444 = ADVANCED_FACE ( 'NONE', ( #3203 ), #1178, .F. ) ;
#1445 = VECTOR ( 'NONE', #6783, 1000.000000000000114 ) ;
#1446 = CARTESIAN_POINT ( 'NONE',  ( -53.78951186480472302, 118.2576901802692788, 47.58386677032791567 ) ) ;
#1447 = CARTESIAN_POINT ( 'NONE',  ( 3.833582208905060185, 166.6352317792379267, 296.5970240496429255 ) ) ;
#1448 = CARTESIAN_POINT ( 'NONE',  ( 19.50571343488122267, 184.8272563654908538, 278.1819008152489232 ) ) ;
#1449 = CARTESIAN_POINT ( 'NONE',  ( -61.06284936382945716, 114.6696180983937410, 168.3840612900001190 ) ) ;
#1450 = CARTESIAN_POINT ( 'NONE',  ( 13.01890817498768449, 190.3110758050131892, 320.8522954438618058 ) ) ;
#1451 = DIRECTION ( 'NONE',  ( 0.7562662552911951774, 0.5735764363510490460, -0.3147561322209052048 ) ) ;
#1452 = CYLINDRICAL_SURFACE ( 'NONE', #9723, 3.399999999999986144 ) ;
#1453 = DIRECTION ( 'NONE',  ( -0.009088227368120101179, -0.7109943316365099353, -0.7031390079522383818 ) ) ;
#1454 = ORIENTED_EDGE ( 'NONE', *, *, #16589, .T. ) ;
#1455 = AXIS2_PLACEMENT_3D ( 'NONE', #6045, #2481, #18131 ) ;
#1456 = PRODUCT_RELATED_PRODUCT_CATEGORY ( 'part', '', ( #7702 ) ) ;
#1457 = CARTESIAN_POINT ( 'NONE',  ( -37.38389485984217941, 95.54566594239412325, 84.82795484212111603 ) ) ;
#1458 = CARTESIAN_POINT ( 'NONE',  ( 48.56920114533915722, 166.9610289984755127, 276.0150354541233924 ) ) ;
#1459 = AXIS2_PLACEMENT_3D ( 'NONE', #6860, #13886, #20874 ) ;
#1460 = ORIENTED_EDGE ( 'NONE', *, *, #7680, .T. ) ;
#1461 = DIRECTION ( 'NONE',  ( -0.5121193912974635332, 0.6668151060996380108, -0.5413791123920870252 ) ) ;
#1462 = ORIENTED_EDGE ( 'NONE', *, *, #2047, .F. ) ;
#1463 = LINE ( 'NONE', #4552, #13309 ) ;
#1464 = PRODUCT_DEFINITION_CONTEXT ( 'detailed design', #20253, 'design' ) ;
#1465 = AXIS2_PLACEMENT_3D ( 'NONE', #17677, #2257, #5695 ) ;
#1466 = DIRECTION ( 'NONE',  ( 0.01292394549866734098, 0.005513023399720419666, 0.9999012842304692006 ) ) ;
#1467 = AXIS2_PLACEMENT_3D ( 'NONE', #15140, #20727, #11671 ) ;
#1468 = CARTESIAN_POINT ( 'NONE',  ( 48.56920114533915722, 166.9610289984755127, 276.0150354541233924 ) ) ;
#1469 = DIRECTION ( 'NONE',  ( 0.008205354412248750534, -0.7726059781012502015, 0.6348327927582032570 ) ) ;
#1470 = ORIENTED_EDGE ( 'NONE', *, *, #22245, .T. ) ;
#1471 = AXIS2_PLACEMENT_3D ( 'NONE', #3974, #14819, #14586 ) ;
#1472 = CARTESIAN_POINT ( 'NONE',  ( 13.55544375494392817, 190.0065045115472913, 320.7925508485532760 ) ) ;
#1473 = CARTESIAN_POINT ( 'NONE',  ( 109.7459976367008636, 75.42189990708665448, 7.816867676514023699 ) ) ;
#1474 =( NAMED_UNIT ( * ) SI_UNIT ( $, .STERADIAN. ) SOLID_ANGLE_UNIT ( ) );
#1475 = CARTESIAN_POINT ( 'NONE',  ( 49.83973329503886873, 168.6466622724117599, 25.96463831280822632 ) ) ;
#1476 = ORIENTED_EDGE ( 'NONE', *, *, #3480, .T. ) ;
#1477 = CARTESIAN_POINT ( 'NONE',  ( 9.466310095025644245, 165.6256992825491068, 113.3939473609682551 ) ) ;
#1478 = EDGE_CURVE ( 'NONE', #9760, #979, #10929, .T. ) ;
#1479 = ORIENTED_EDGE ( 'NONE', *, *, #22347, .F. ) ;
#1480 = FACE_OUTER_BOUND ( 'NONE', #8854, .T. ) ;
#1481 = CARTESIAN_POINT ( 'NONE',  ( 68.71681667565954399, 72.00000000000000000, -85.89527988174788220 ) ) ;
#1482 = CIRCLE ( 'NONE', #4394, 2.499999999999988010 ) ;
#1483 = APPLICATION_CONTEXT ( 'automotive_design' ) ;
#1484 = DIRECTION ( 'NONE',  ( -0.01292394549866632963, -0.005513023399716958026, -0.9999012842304692006 ) ) ;
#1485 = DIRECTION ( 'NONE',  ( -0.6979091139780387865, 0.003898296230782432540, 0.7161757269782926816 ) ) ;
#1486 = AXIS2_PLACEMENT_3D ( 'NONE', #6155, #18132, #5923 ) ;
#1487 = FACE_BOUND ( 'NONE', #13024, .T. ) ;
#1488 = CARTESIAN_POINT ( 'NONE',  ( -41.47069032946998846, 166.0668615304125808, 273.1833561390217824 ) ) ;
#1489 = EDGE_CURVE ( 'NONE', #21811, #4404, #4303, .T. ) ;
#1490 = EDGE_LOOP ( 'NONE', ( #11140, #6674, #21508, #8387 ) ) ;
#1491 = EDGE_CURVE ( 'NONE', #19968, #18675, #13691, .T. ) ;
#1492 = FACE_OUTER_BOUND ( 'NONE', #20573, .T. ) ;
#1493 = CARTESIAN_POINT ( 'NONE',  ( -45.88247808544533513, 166.6336875933314161, 269.2368593367144740 ) ) ;
#1494 = CARTESIAN_POINT ( 'NONE',  ( 64.99457118636310327, 170.0000000000000284, -0.8400692238017243296 ) ) ;
#1495 = LINE ( 'NONE', #6987, #15156 ) ;
#1496 = AXIS2_PLACEMENT_3D ( 'NONE', #10517, #5668, #10619 ) ;
#1497 = DIRECTION ( 'NONE',  ( -0.01292394549866632963, -0.005513023399716958026, -0.9999012842304692006 ) ) ;
#1498 = PRODUCT_DEFINITION_SHAPE ( 'NONE', 'NONE',  #22684 ) ;
#1499 = DIRECTION ( 'NONE',  ( -0.01292414190463832269, 0.000000000000000000, -0.9999164797902017066 ) ) ;
#1500 = VECTOR ( 'NONE', #10868, 1000.000000000000000 ) ;
#1501 = EDGE_LOOP ( 'NONE', ( #17646, #17489, #7558, #20601, #8372, #14963, #15263, #20562, #9434, #13836, #9394, #3686, #8049, #16135, #18646, #21048, #4801, #16875, #2262, #19730, #15751 ) ) ;
#1502 = CARTESIAN_POINT ( 'NONE',  ( 49.81003579750536403, 110.5281110817785049, -47.59029815665551411 ) ) ;
#1503 = ORIENTED_EDGE ( 'NONE', *, *, #12891, .T. ) ;
#1504 = DIRECTION ( 'NONE',  ( 0.7912924530843117310, -0.6113994113550570431, -0.006856638134102506846 ) ) ;
#1505 = AXIS2_PLACEMENT_3D ( 'NONE', #20426, #11715, #2979 ) ;
#1506 = CARTESIAN_POINT ( 'NONE',  ( -86.79222083800951282, 104.3814432989690602, -67.58039954014913064 ) ) ;
#1507 = CARTESIAN_POINT ( 'NONE',  ( -48.59258154118273865, 108.3707227317548529, -45.53672366955343165 ) ) ;
#1508 = CARTESIAN_POINT ( 'NONE',  ( 19.46461987976676511, 177.6255169206013989, 113.1985551865116406 ) ) ;
#1509 = EDGE_CURVE ( 'NONE', #848, #22315, #10189, .T. ) ;
#1510 = DIRECTION ( 'NONE',  ( 0.9999164797902017066, 2.001050586450178695E-22, -0.01292414190464131508 ) ) ;
#1511 = CARTESIAN_POINT ( 'NONE',  ( -41.96503124479402658, 165.8559883853732515, 234.9371320172060678 ) ) ;
#1512 = AXIS2_PLACEMENT_3D ( 'NONE', #12811, #16166, #19461 ) ;
#1513 = ORIENTED_EDGE ( 'NONE', *, *, #20558, .T. ) ;
#1514 = CARTESIAN_POINT ( 'NONE',  ( -14.93612093091044102, 185.1121758471145142, 276.7357782268812798 ) ) ;
#1515 = ADVANCED_FACE ( 'NONE', ( #5036 ), #19055, .T. ) ;
#1516 = DIRECTION ( 'NONE',  ( -5.440186201345785633E-18, -1.000000000000000000, -1.334940939666367878E-17 ) ) ;
#1517 = ORIENTED_EDGE ( 'NONE', *, *, #11816, .T. ) ;
#1518 = CARTESIAN_POINT ( 'NONE',  ( 39.42082737383937996, 91.17157287525388654, -83.51645567887783272 ) ) ;
#1519 = AXIS2_PLACEMENT_3D ( 'NONE', #9593, #754, #11427 ) ;
#1520 = CARTESIAN_POINT ( 'NONE',  ( -88.16443613784075239, 88.35912761021998563, 52.83007831909758067 ) ) ;
#1521 = VECTOR ( 'NONE', #6569, 1000.000000000000000 ) ;
#1522 = EDGE_LOOP ( 'NONE', ( #6462, #16819, #9996, #12609 ) ) ;
#1523 = EDGE_CURVE ( 'NONE', #9064, #5658, #4596, .T. ) ;
#1524 = ORIENTED_EDGE ( 'NONE', *, *, #4986, .T. ) ;
#1525 = DIRECTION ( 'NONE',  ( 7.125109674364536131E-05, -0.9999848031710253382, 0.005512562950849705760 ) ) ;
#1526 = STYLED_ITEM ( 'NONE', ( #11230 ), #9502 ) ;
#1527 = CARTESIAN_POINT ( 'NONE',  ( -34.80083724429680814, 171.3633268630252644, 247.7587566398530612 ) ) ;
#1528 = CARTESIAN_POINT ( 'NONE',  ( -20.68543912716607736, 88.27010240781663697, -77.04715649662465182 ) ) ;
#1529 = ORIENTED_EDGE ( 'NONE', *, *, #21240, .F. ) ;
#1530 = CARTESIAN_POINT ( 'NONE',  ( 83.79153344593285624, 75.05951099091890910, -4.453614549308245962 ) ) ;
#1531 = CARTESIAN_POINT ( 'NONE',  ( -70.91392079944854743, 91.32005360614647316, -84.09052168258642723 ) ) ;
#1532 = VERTEX_POINT ( 'NONE', #21232 ) ;
#1533 = EDGE_LOOP ( 'NONE', ( #16762, #10478, #19295 ) ) ;
#1534 = FACE_OUTER_BOUND ( 'NONE', #12231, .T. ) ;
#1535 = CARTESIAN_POINT ( 'NONE',  ( 10.04616666026851313, 189.9867745584397767, 275.0214033402720588 ) ) ;
#1536 = DIRECTION ( 'NONE',  ( 0.8981428216242028917, -0.000000000000000000, 0.4397038457472429718 ) ) ;
#1537 = DIRECTION ( 'NONE',  ( 0.9999464000778710560, 1.417269118681125921E-05, -0.01035358732233959689 ) ) ;
#1538 = AXIS2_PLACEMENT_3D ( 'NONE', #8085, #15121, #22073 ) ;
#1539 = CARTESIAN_POINT ( 'NONE',  ( -12.04904146786470776, 146.2738556374876282, 276.7751546531125655 ) ) ;
#1540 =( GEOMETRIC_REPRESENTATION_CONTEXT ( 3 ) GLOBAL_UNCERTAINTY_ASSIGNED_CONTEXT ( ( #813 ) ) GLOBAL_UNIT_ASSIGNED_CONTEXT ( ( #17647, #10405, #3847 ) ) REPRESENTATION_CONTEXT ( 'NONE', 'WORKASPACE' ) );
#1541 = VECTOR ( 'NONE', #19976, 999.9999999999998863 ) ;
#1542 = EDGE_CURVE ( 'NONE', #8847, #14836, #288, .T. ) ;
#1543 = VECTOR ( 'NONE', #20457, 1000.000000000000000 ) ;
#1544 = CARTESIAN_POINT ( 'NONE',  ( 12.39776786404130782, 161.0697644098447370, 324.5197799491688215 ) ) ;
#1545 = ORIENTED_EDGE ( 'NONE', *, *, #2061, .T. ) ;
#1546 = ORIENTED_EDGE ( 'NONE', *, *, #3211, .T. ) ;
#1547 = CARTESIAN_POINT ( 'NONE',  ( 47.42517700970201133, 109.3838229944194609, -44.78316280508298775 ) ) ;
#1548 = TOROIDAL_SURFACE ( 'NONE', #1905, 20.50000000000000355, 2.000000000000000000 ) ;
#1549 = ORIENTED_EDGE ( 'NONE', *, *, #6294, .F. ) ;
#1550 = VECTOR ( 'NONE', #4109, 1000.000000000000114 ) ;
#1551 = EDGE_CURVE ( 'NONE', #9056, #6260, #1727, .T. ) ;
#1552 = CARTESIAN_POINT ( 'NONE',  ( 0.000000000000000000, 25.00000000000000000, 0.000000000000000000 ) ) ;
#1553 = CARTESIAN_POINT ( 'NONE',  ( -90.06393689865117835, 72.00000000000000000, 59.85988923254397776 ) ) ;
#1554 = PLANE ( 'NONE',  #3802 ) ;
#1555 = CARTESIAN_POINT ( 'NONE',  ( -91.62437796271723300, 71.80839515725416788, -60.86849236629029036 ) ) ;
#1556 = VECTOR ( 'NONE', #13048, 1000.000000000000114 ) ;
#1557 = PLANE ( 'NONE',  #13925 ) ;
#1558 = CARTESIAN_POINT ( 'NONE',  ( 163.1715728752537018, 20.00000000000000355, -8.828427124748447596 ) ) ;
#1559 = CARTESIAN_POINT ( 'NONE',  ( 58.87600894486503478, 126.5883500096209815, 106.0876318414197499 ) ) ;
#1560 = CARTESIAN_POINT ( 'NONE',  ( 11.78290328754079219, 187.7711080693391921, 304.8720351003711357 ) ) ;
#1561 = LINE ( 'NONE', #13631, #6036 ) ;
#1562 = DIRECTION ( 'NONE',  ( -0.01292414190464022741, 0.000000000000000000, -0.9999164797902017066 ) ) ;
#1563 = AXIS2_PLACEMENT_3D ( 'NONE', #15805, #5850, #3494 ) ;
#1564 = CIRCLE ( 'NONE', #16995, 8.000000000000000000 ) ;
#1565 = ADVANCED_FACE ( 'NONE', ( #19625 ), #12400, .T. ) ;
#1566 = DIRECTION ( 'NONE',  ( 0.000000000000000000, 1.000000000000000000, 0.000000000000000000 ) ) ;
#1567 = DIRECTION ( 'NONE',  ( 0.01292394549866738782, 0.005513023399720468239, 0.9999012842304692006 ) ) ;
#1568 = ADVANCED_FACE ( 'NONE', ( #5152 ), #15756, .T. ) ;
#1569 = EDGE_LOOP ( 'NONE', ( #12182, #20918, #6623 ) ) ;
#1570 = CARTESIAN_POINT ( 'NONE',  ( -89.22443767324087105, 80.23075532867244419, -29.93879111800710646 ) ) ;
#1571 = VERTEX_POINT ( 'NONE', #2067 ) ;
#1572 = ORIENTED_EDGE ( 'NONE', *, *, #3820, .T. ) ;
#1573 = VECTOR ( 'NONE', #11501, 1000.000000000000000 ) ;
#1574 = DIRECTION ( 'NONE',  ( -7.125109674160325297E-05, 0.9999848031710253382, -0.005512562950849327591 ) ) ;
#1575 = AXIS2_PLACEMENT_3D ( 'NONE', #11584, #21774, #9508 ) ;
#1576 = AXIS2_PLACEMENT_3D ( 'NONE', #20398, #18806, #9968 ) ;
#1577 = CARTESIAN_POINT ( 'NONE',  ( 45.44318007003697346, 173.1906980738791617, 33.99720069194405170 ) ) ;
#1578 = SPHERICAL_SURFACE ( 'NONE', #14052, 11.00000000000000533 ) ;
#1579 = EDGE_LOOP ( 'NONE', ( #18293, #4104, #6095, #706 ) ) ;
#1580 = CARTESIAN_POINT ( 'NONE',  ( 55.40268456415107323, 20.00000000000000000, -113.1659955246503557 ) ) ;
#1581 = VERTEX_POINT ( 'NONE', #10459 ) ;
#1582 = ORIENTED_EDGE ( 'NONE', *, *, #10898, .F. ) ;
#1583 = DIRECTION ( 'NONE',  ( 7.125109674160325297E-05, -0.9999848031710253382, 0.005512562950849327591 ) ) ;
#1584 = CARTESIAN_POINT ( 'NONE',  ( 48.56920114533915722, 166.9610289984755127, 276.0150354541233924 ) ) ;
#1585 = SURFACE_STYLE_FILL_AREA ( #10197 ) ;
#1586 = DIRECTION ( 'NONE',  ( -0.7938906895485154935, 0.003295407061475229184, 0.6080515712836221942 ) ) ;
#1587 = EDGE_LOOP ( 'NONE', ( #2535, #7607 ) ) ;
#1588 = CARTESIAN_POINT ( 'NONE',  ( 39.66847363096314893, 93.56461422141673268, 82.92963109642391828 ) ) ;
#1589 = ORIENTED_EDGE ( 'NONE', *, *, #17013, .T. ) ;
#1590 = DIRECTION ( 'NONE',  ( 0.000000000000000000, 0.000000000000000000, 1.000000000000000000 ) ) ;
#1591 = CARTESIAN_POINT ( 'NONE',  ( 157.5176307659770885, 20.00000000000000000, -60.94675664190840081 ) ) ;
#1592 = AXIS2_PLACEMENT_3D ( 'NONE', #10762, #9016, #16064 ) ;
#1593 = CIRCLE ( 'NONE', #11489, 2.000000000000005329 ) ;
#1594 = CARTESIAN_POINT ( 'NONE',  ( 14.92693155316947262, 186.3292256045772604, 305.6379776027275170 ) ) ;
#1595 = CARTESIAN_POINT ( 'NONE',  ( -55.33837949231439524, 118.9192529882355984, 167.6120857178885899 ) ) ;
#1596 = ORIENTED_EDGE ( 'NONE', *, *, #4557, .T. ) ;
#1597 = CARTESIAN_POINT ( 'NONE',  ( -49.64993871177497198, 140.1470898690141098, 27.40669857513504226 ) ) ;
#1598 = DIRECTION ( 'NONE',  ( 0.01292394549866738782, 0.005513023399720468239, 0.9999012842304692006 ) ) ;
#1599 = LINE ( 'NONE', #5474, #11835 ) ;
#1600 = CONTEXT_DEPENDENT_SHAPE_REPRESENTATION ( #22150, #20367 ) ;
#1601 = CARTESIAN_POINT ( 'NONE',  ( 18.69536052806381576, 189.4444907833431273, -101.0667417618364965 ) ) ;
#1602 = VECTOR ( 'NONE', #19277, 1000.000000000000114 ) ;
#1603 = AXIS2_PLACEMENT_3D ( 'NONE', #9229, #4388, #14895 ) ;
#1604 = ORIENTED_EDGE ( 'NONE', *, *, #10918, .T. ) ;
#1605 = PLANE ( 'NONE',  #17716 ) ;
#1606 = LINE ( 'NONE', #15865, #11517 ) ;
#1607 = CARTESIAN_POINT ( 'NONE',  ( 64.42259306105445660, 139.7551263635816952, -45.17031240767400391 ) ) ;
#1608 = FACE_OUTER_BOUND ( 'NONE', #14068, .T. ) ;
#1609 = CIRCLE ( 'NONE', #16669, 8.000000000000003553 ) ;
#1610 = ORIENTED_EDGE ( 'NONE', *, *, #13094, .F. ) ;
#1611 = CARTESIAN_POINT ( 'NONE',  ( 8.492591494844877076, 81.64068272718454011, -90.21500375438164099 ) ) ;
#1612 = AXIS2_PLACEMENT_3D ( 'NONE', #16636, #16404, #21423 ) ;
#1613 = CARTESIAN_POINT ( 'NONE',  ( 91.62437796271727564, 34.61572286322119396, 60.86849236629024773 ) ) ;
#1614 = VERTEX_POINT ( 'NONE', #5267 ) ;
#1615 = CARTESIAN_POINT ( 'NONE',  ( -89.50333764702355666, 88.30151482414257202, 50.59770125036460797 ) ) ;
#1616 = EDGE_LOOP ( 'NONE', ( #15461, #11092, #3428 ) ) ;
#1617 = DIRECTION ( 'NONE',  ( 0.8981428216242088869, -0.000000000000000000, 0.4397038457472307593 ) ) ;
#1618 = PLANE ( 'NONE',  #19237 ) ;
#1619 = CARTESIAN_POINT ( 'NONE',  ( 79.99331838321626265, 102.0000000000000000, -1.033931352371318058 ) ) ;
#1620 = CARTESIAN_POINT ( 'NONE',  ( -40.31377174949672337, 163.2475007341206776, 273.1839474467614650 ) ) ;
#1621 = DIRECTION ( 'NONE',  ( -7.125109674243555432E-05, 0.9999848031710253382, -0.005512562950850175003 ) ) ;
#1622 = DIRECTION ( 'NONE',  ( 0.000000000000000000, -1.000000000000000000, 0.000000000000000000 ) ) ;
#1623 = VECTOR ( 'NONE', #1863, 1000.000000000000114 ) ;
#1624 = ADVANCED_FACE ( 'NONE', ( #12415 ), #9070, .T. ) ;
#1625 = EDGE_LOOP ( 'NONE', ( #5052, #16017, #17901, #17803 ) ) ;
#1626 = CARTESIAN_POINT ( 'NONE',  ( -0.4408429396002318534, 81.99999999999998579, -98.97428162928156326 ) ) ;
#1627 = VERTEX_POINT ( 'NONE', #2968 ) ;
#1628 = VECTOR ( 'NONE', #7640, 999.9999999999998863 ) ;
#1629 = AXIS2_PLACEMENT_3D ( 'NONE', #3300, #13778, #10441 ) ;
#1630 = CARTESIAN_POINT ( 'NONE',  ( 90.07355500607899046, 71.53834005368396731, -63.14076745314238792 ) ) ;
#1631 = CARTESIAN_POINT ( 'NONE',  ( -88.16398599203232322, 88.31536494695383510, 52.86903560245924183 ) ) ;
#1632 = DIRECTION ( 'NONE',  ( -0.01292394549866727679, -0.005513023399720742325, -0.9999012842304692006 ) ) ;
#1633 = EDGE_LOOP ( 'NONE', ( #20805, #14604, #13579, #1411 ) ) ;
#1634 = ADVANCED_FACE ( 'NONE', ( #19289 ), #5393, .F. ) ;
#1635 = EDGE_LOOP ( 'NONE', ( #7699, #12746 ) ) ;
#1636 = CARTESIAN_POINT ( 'NONE',  ( -12.58378492319879527, 109.7167104967248434, 130.3428598364639299 ) ) ;
#1637 = FACE_OUTER_BOUND ( 'NONE', #10344, .T. ) ;
#1638 = CARTESIAN_POINT ( 'NONE',  ( 1.717753310876221295, 45.00000000000000000, 109.6869605904137330 ) ) ;
#1639 = CIRCLE ( 'NONE', #20337, 110.5324305509042233 ) ;
#1640 = CARTESIAN_POINT ( 'NONE',  ( 0.000000000000000000, 45.00000000000000711, 0.000000000000000000 ) ) ;
#1641 = B_SPLINE_CURVE_WITH_KNOTS ( 'NONE', 3,
 ( #11508, #20333, #14964, #2985, #2774, #14862, #19984, #1292 ),
 .UNSPECIFIED., .F., .F.,
 ( 4, 2, 2, 4 ),
 ( 6.938893903907228378E-18, 0.001422831528841437491, 0.002134247293262152984, 0.002845663057682868043 ),
 .UNSPECIFIED. ) ;
#1642 = DIRECTION ( 'NONE',  ( -0.9999164797902015955, -6.965998958219364448E-18, 0.01292414190464157182 ) ) ;
#1643 = CARTESIAN_POINT ( 'NONE',  ( -44.86761910970069778, 151.3223208568695952, 257.3069776102678929 ) ) ;
#1644 = ORIENTED_EDGE ( 'NONE', *, *, #7964, .T. ) ;
#1645 = EDGE_CURVE ( 'NONE', #4445, #13100, #6158, .T. ) ;
#1646 = ORIENTED_EDGE ( 'NONE', *, *, #16659, .F. ) ;
#1647 = CARTESIAN_POINT ( 'NONE',  ( -11.78710887361312132, 185.2757727756024622, 278.4447062962351538 ) ) ;
#1648 = DIRECTION ( 'NONE',  ( 0.1136178953597579561, -0.9935164314186356593, 0.004009283626633663132 ) ) ;
#1649 = CARTESIAN_POINT ( 'NONE',  ( -11.46885069223597853, 70.80384757729338219, -91.33151364841882014 ) ) ;
#1650 = CARTESIAN_POINT ( 'NONE',  ( -40.73497377069196546, 95.07629454920768808, 83.32674675967490430 ) ) ;
#1651 = VECTOR ( 'NONE', #15859, 999.9999999999998863 ) ;
#1652 = DIRECTION ( 'NONE',  ( 0.9999164797902015955, 6.965998958219364448E-18, -0.01292414190464157182 ) ) ;
#1653 = VERTEX_POINT ( 'NONE', #14382 ) ;
#1654 = DIRECTION ( 'NONE',  ( 0.000000000000000000, 0.000000000000000000, 1.000000000000000000 ) ) ;
#1655 = DIRECTION ( 'NONE',  ( 0.01220060921879500236, -0.3298969072164960603, 0.9439381207174974975 ) ) ;
#1656 = CARTESIAN_POINT ( 'NONE',  ( 105.4170939775132894, 71.46263312473240603, -31.42050039360495006 ) ) ;
#1657 = EDGE_CURVE ( 'NONE', #18197, #21410, #21895, .T. ) ;
#1658 = EDGE_CURVE ( 'NONE', #22201, #6614, #2119, .T. ) ;
#1659 = ADVANCED_FACE ( 'NONE', ( #8831 ), #3447, .F. ) ;
#1660 = CARTESIAN_POINT ( 'NONE',  ( -157.5176307659779411, 0.000000000000000000, 60.94675664190622655 ) ) ;
#1661 = ORIENTED_EDGE ( 'NONE', *, *, #3227, .T. ) ;
#1662 = AXIS2_PLACEMENT_3D ( 'NONE', #19654, #14289, #2098 ) ;
#1663 = ORIENTED_EDGE ( 'NONE', *, *, #8994, .T. ) ;
#1664 = VERTEX_POINT ( 'NONE', #17478 ) ;
#1665 = ADVANCED_FACE ( 'NONE', ( #14150 ), #3943, .T. ) ;
#1666 = UNCERTAINTY_MEASURE_WITH_UNIT (LENGTH_MEASURE( 1.000000000000000082E-05 ), #7282, 'distance_accuracy_value', 'NONE');
#1667 = FACE_OUTER_BOUND ( 'NONE', #18510, .T. ) ;
#1668 = ORIENTED_EDGE ( 'NONE', *, *, #1017, .F. ) ;
#1669 = LINE ( 'NONE', #7270, #16480 ) ;
#1670 = CARTESIAN_POINT ( 'NONE',  ( 50.34270678259964882, 126.1473026246199254, 26.19146026598277643 ) ) ;
#1671 = EDGE_CURVE ( 'NONE', #14389, #20401, #13864, .T. ) ;
#1672 = DIRECTION ( 'NONE',  ( -5.440186201345785633E-18, -1.000000000000000000, -1.334940939666367878E-17 ) ) ;
#1673 = CARTESIAN_POINT ( 'NONE',  ( 51.43549903698337999, 154.9275132768233618, 276.0443355225219761 ) ) ;
#1674 = ADVANCED_FACE ( 'NONE', ( #10680 ), #1765, .T. ) ;
#1675 =( NAMED_UNIT ( * ) PLANE_ANGLE_UNIT ( ) SI_UNIT ( $, .RADIAN. ) );
#1676 = VECTOR ( 'NONE', #17134, 1000.000000000000114 ) ;
#1677 = CARTESIAN_POINT ( 'NONE',  ( 86.06478871700173272, 75.01038043515919185, -2.531004044634442174 ) ) ;
#1678 = CARTESIAN_POINT ( 'NONE',  ( 11.82873084905181749, 187.7848449878356405, 307.7666980689497791 ) ) ;
#1679 = CARTESIAN_POINT ( 'NONE',  ( 33.82085273160093664, 93.50464841319750064, -82.93470554904388337 ) ) ;
#1680 = CARTESIAN_POINT ( 'NONE',  ( -55.98629706596215527, 114.1919480473872852, 162.6802715674982664 ) ) ;
#1681 = ORIENTED_EDGE ( 'NONE', *, *, #19106, .T. ) ;
#1682 = SHAPE_REPRESENTATION_RELATIONSHIP ( 'NONE' , 'NONE' ,  #3137, #19759 ) ;
#1683 = EDGE_CURVE ( 'NONE', #11404, #11011, #10571, .T. ) ;
#1684 = CARTESIAN_POINT ( 'NONE',  ( 3.316624388958365088, 166.4147108432491109, 256.6009726804241495 ) ) ;
#1685 = DIRECTION ( 'NONE',  ( -0.8981428216242028917, -0.000000000000000000, -0.4397038457472429718 ) ) ;
#1686 = ORIENTED_EDGE ( 'NONE', *, *, #9145, .F. ) ;
#1687 = CARTESIAN_POINT ( 'NONE',  ( 0.000000000000000000, 20.00000000000000000, 0.000000000000000000 ) ) ;
#1688 = ORIENTED_EDGE ( 'NONE', *, *, #1509, .F. ) ;
#1689 = B_SPLINE_CURVE_WITH_KNOTS ( 'NONE', 3,
 ( #12813, #20028, #11315, #11410, #21726, #18300, #21937, #13260, #7736, #9448, #4165, #2568 ),
 .UNSPECIFIED., .F., .F.,
 ( 4, 2, 2, 2, 2, 4 ),
 ( 0.000000000000000000, 0.003508523874122987905, 0.007017047748245975811, 0.01052557162236896285, 0.01227983355943044162, 0.01403409549649192040 ),
 .UNSPECIFIED. ) ;
#1690 = VECTOR ( 'NONE', #4472, 1000.000000000000227 ) ;
#1691 = DIRECTION ( 'NONE',  ( -0.01292394549866745720, -0.005513023399720816918, -0.9999012842304692006 ) ) ;
#1692 = VERTEX_POINT ( 'NONE', #19518 ) ;
#1693 = CYLINDRICAL_SURFACE ( 'NONE', #7075, 8.000000000000003553 ) ;
#1694 = CARTESIAN_POINT ( 'NONE',  ( 16.39796002119450335, 145.1381702172243706, 275.9805542436448036 ) ) ;
#1695 = EDGE_CURVE ( 'NONE', #20021, #12292, #10809, .T. ) ;
#1696 = ORIENTED_EDGE ( 'NONE', *, *, #16280, .F. ) ;
#1697 = CARTESIAN_POINT ( 'NONE',  ( 64.31463902574824942, 189.7102623349352086, -53.44513790491837568 ) ) ;
#1698 = ORIENTED_EDGE ( 'NONE', *, *, #13573, .F. ) ;
#1699 = CARTESIAN_POINT ( 'NONE',  ( 51.17420407245305825, 179.0367939709223606, 273.9145872160426620 ) ) ;
#1700 = CARTESIAN_POINT ( 'NONE',  ( -39.60774975246459917, 168.4783572853436624, 273.1459812745235354 ) ) ;
#1701 = CARTESIAN_POINT ( 'NONE',  ( 3.872354045398203937, 166.6517708494369856, 299.5967279023338392 ) ) ;
#1702 = CARTESIAN_POINT ( 'NONE',  ( 9.143198533613464463, 165.4878681845327151, 88.39541535392230287 ) ) ;
#1703 = VERTEX_POINT ( 'NONE', #20071 ) ;
#1704 = LINE ( 'NONE', #11119, #17313 ) ;
#1705 = CARTESIAN_POINT ( 'NONE',  ( -12.64660359835458792, 105.6831695174542745, 124.2703293933457758 ) ) ;
#1706 = CARTESIAN_POINT ( 'NONE',  ( 17.30323760145302714, 177.5566041281049081, 100.7256374174400548 ) ) ;
#1707 = CARTESIAN_POINT ( 'NONE',  ( -41.84548474893134085, 165.9069838518206836, 244.1862188963381755 ) ) ;
#1708 = CARTESIAN_POINT ( 'NONE',  ( 20.16650508637343719, 182.5115947525307263, 317.5179922051294739 ) ) ;
#1709 = CARTESIAN_POINT ( 'NONE',  ( -1.885502603235176045, 70.00000000000001421, -81.01068473295498507 ) ) ;
#1710 = DIRECTION ( 'NONE',  ( -0.008899921406766564749, 0.7251151399516315710, -0.6885701309321218266 ) ) ;
#1711 = CARTESIAN_POINT ( 'NONE',  ( 41.19649195735513558, 119.7615706795621691, 247.0609841073601842 ) ) ;
#1712 = DIRECTION ( 'NONE',  ( 0.01292394549866739996, 0.005513023399721131770, 0.9999012842304692006 ) ) ;
#1713 = CARTESIAN_POINT ( 'NONE',  ( 18.38499007693353349, 64.93155780410931754, -125.0795181004832415 ) ) ;
#1714 = DIRECTION ( 'NONE',  ( 0.000000000000000000, 0.000000000000000000, 1.000000000000000000 ) ) ;
#1715 = DIRECTION ( 'NONE',  ( 0.01292394549866740169, 0.005513023399720822990, 0.9999012842304693116 ) ) ;
#1716 = EDGE_CURVE ( 'NONE', #20174, #6772, #18260, .T. ) ;
#1717 = CARTESIAN_POINT ( 'NONE',  ( -56.14669609475481593, 126.5745674511214673, 105.0741549498773679 ) ) ;
#1718 = EDGE_CURVE ( 'NONE', #8332, #1333, #21667, .T. ) ;
#1719 = DIRECTION ( 'NONE',  ( 0.9999164797902015955, 0.000000000000000000, -0.01292414190463754553 ) ) ;
#1720 = VERTEX_POINT ( 'NONE', #9293 ) ;
#1721 = DIRECTION ( 'NONE',  ( 0.000000000000000000, 0.000000000000000000, 1.000000000000000000 ) ) ;
#1722 = CARTESIAN_POINT ( 'NONE',  ( 0.000000000000000000, 29.00000000000000711, -78.99999999999998579 ) ) ;
#1723 = ORIENTED_EDGE ( 'NONE', *, *, #22453, .T. ) ;
#1724 = CARTESIAN_POINT ( 'NONE',  ( -89.68778923927422397, 88.14345933540539590, 50.69680520791115441 ) ) ;
#1725 = VERTEX_POINT ( 'NONE', #5958 ) ;
#1726 = CARTESIAN_POINT ( 'NONE',  ( 106.6839260360358992, 79.12661604778581648, 26.80604816241556065 ) ) ;
#1727 = LINE ( 'NONE', #3893, #20440 ) ;
#1728 = DIRECTION ( 'NONE',  ( 0.9999164797902015955, 0.000000000000000000, -0.01292414190464174703 ) ) ;
#1729 = ORIENTED_EDGE ( 'NONE', *, *, #10659, .T. ) ;
#1730 = FACE_OUTER_BOUND ( 'NONE', #6402, .T. ) ;
#1731 = CARTESIAN_POINT ( 'NONE',  ( 91.23603883849617091, 69.99999999999998579, 30.82342686631245954 ) ) ;
#1732 = ORIENTED_EDGE ( 'NONE', *, *, #3168, .F. ) ;
#1733 = PRODUCT_RELATED_PRODUCT_CATEGORY ( 'part', '', ( #16535 ) ) ;
#1734 = CARTESIAN_POINT ( 'NONE',  ( 0.3064506171779977084, 327.3432411309900090, 313.2566634950479170 ) ) ;
#1735 = CARTESIAN_POINT ( 'NONE',  ( 21.71998689217155132, 185.4674263880815204, 276.2600312189053966 ) ) ;
#1736 = ORIENTED_EDGE ( 'NONE', *, *, #10040, .F. ) ;
#1737 = LINE ( 'NONE', #17598, #21237 ) ;
#1738 = CARTESIAN_POINT ( 'NONE',  ( -88.17040607254148199, 88.78744216278629153, 52.26814626353031912 ) ) ;
#1739 = DIRECTION ( 'NONE',  ( 0.009138748381789079875, 0.7071067811865487940, 0.7070477234798316912 ) ) ;
#1741 = ORIENTED_EDGE ( 'NONE', *, *, #16059, .F. ) ;
#1740 = ORIENTED_EDGE ( 'NONE', *, *, #7164, .T. ) ;
#1742 = EDGE_LOOP ( 'NONE', ( #11477, #2679, #19385, #12838 ) ) ;
#1743 = LINE ( 'NONE', #3677, #16966 ) ;
#1744 = DIRECTION ( 'NONE',  ( 0.9909299940865187173, -0.1338359446631173233, -0.01207007604876291287 ) ) ;
#1745 = VERTEX_POINT ( 'NONE', #14718 ) ;
#1746 = ADVANCED_FACE ( 'NONE', ( #16551 ), #805, .F. ) ;
#1747 = CARTESIAN_POINT ( 'NONE',  ( 83.41173289365072208, 75.07748563434969924, 2.765778341857892730 ) ) ;
#1748 = CIRCLE ( 'NONE', #16801, 10.99999999999999289 ) ;
#1749 = DIRECTION ( 'NONE',  ( 0.9232306267972774094, 0.000000000000000000, -0.3842462878721227826 ) ) ;
#1750 = ORIENTED_EDGE ( 'NONE', *, *, #1372, .T. ) ;
#1751 = EDGE_LOOP ( 'NONE', ( #22660, #6335, #2230, #5340 ) ) ;
#1752 = CARTESIAN_POINT ( 'NONE',  ( -88.41758806590422637, 80.31838830481380853, 32.48564084813592956 ) ) ;
#1753 = CARTESIAN_POINT ( 'NONE',  ( -75.54218441871489631, 75.03417954463952810, 3.529018660298018695 ) ) ;
#1754 = CARTESIAN_POINT ( 'NONE',  ( -8.905365697803494740, 165.2773500475165065, 321.1137824091954940 ) ) ;
#1755 = CARTESIAN_POINT ( 'NONE',  ( 90.02055463237803679, 72.00000000000000000, -63.21629334023821656 ) ) ;
#1756 = ORIENTED_EDGE ( 'NONE', *, *, #14559, .T. ) ;
#1757 = CARTESIAN_POINT ( 'NONE',  ( -93.21002351426726307, 72.00000000000000000, -28.79774562292281104 ) ) ;
#1758 = LINE ( 'NONE', #31, #17434 ) ;
#1759 = CARTESIAN_POINT ( 'NONE',  ( 104.9011368644396782, 70.01236949047483904, -33.10239539927077601 ) ) ;
#1760 = ORIENTED_EDGE ( 'NONE', *, *, #14884, .F. ) ;
#1761 = EDGE_CURVE ( 'NONE', #4814, #10791, #21560, .T. ) ;
#1762 = DIRECTION ( 'NONE',  ( 0.9999164797902015955, 6.965998958219364448E-18, -0.01292414190464157182 ) ) ;
#1763 = ORIENTED_EDGE ( 'NONE', *, *, #15678, .T. ) ;
#1764 = ORIENTED_EDGE ( 'NONE', *, *, #2080, .T. ) ;
#1765 = CONICAL_SURFACE ( 'NONE', #4670, 9.000000000000001776, 1.047197551196594301 ) ;
#1766 = DIRECTION ( 'NONE',  ( 0.01292414190464174703, 0.000000000000000000, 0.9999164797902015955 ) ) ;
#1767 = ADVANCED_FACE ( 'NONE', ( #19961 ), #10909, .F. ) ;
#1768 = ORIENTED_EDGE ( 'NONE', *, *, #22239, .T. ) ;
#1769 = DIRECTION ( 'NONE',  ( 7.125109674403276030E-05, -0.9999848031710252272, 0.005512562950848280685 ) ) ;
#1770 = CARTESIAN_POINT ( 'NONE',  ( -90.58204872677625019, 70.40262524007013667, 62.40924858436775935 ) ) ;
#1771 = CARTESIAN_POINT ( 'NONE',  ( -3.701274867523290713, 143.2855812733562288, 275.7914880546696281 ) ) ;
#1772 = CIRCLE ( 'NONE', #5048, 6.499999999999998224 ) ;
#1773 = EDGE_CURVE ( 'NONE', #22552, #13067, #11786, .T. ) ;
#1774 = DIRECTION ( 'NONE',  ( -0.000000000000000000, -1.000000000000000000, -0.000000000000000000 ) ) ;
#1775 = CARTESIAN_POINT ( 'NONE',  ( -14.02864438394168722, 325.7329298795136197, 320.4531201330285626 ) ) ;
#1776 = EDGE_CURVE ( 'NONE', #19048, #15773, #9846, .T. ) ;
#1777 = ORIENTED_EDGE ( 'NONE', *, *, #3040, .T. ) ;
#1778 = SURFACE_STYLE_USAGE ( .BOTH. , #5432 ) ;
#1779 = CARTESIAN_POINT ( 'NONE',  ( 84.91452901814238885, 75.07584193902901859, -4.908336678377503759 ) ) ;
#1780 = CARTESIAN_POINT ( 'NONE',  ( 14.12971913360413367, 189.6478225779368358, 308.0282301501843563 ) ) ;
#1781 = CARTESIAN_POINT ( 'NONE',  ( 91.97397837737798909, 77.39048292941922114, 29.24031187446957958 ) ) ;
#1782 = AXIS2_PLACEMENT_3D ( 'NONE', #17932, #2168, #5721 ) ;
#1783 = DIRECTION ( 'NONE',  ( 2.025474946048326158E-22, -1.000000000000000000, 1.876735158486679638E-22 ) ) ;
#1784 = EDGE_CURVE ( 'NONE', #10110, #15773, #14258, .T. ) ;
#1785 = DIRECTION ( 'NONE',  ( 0.9999164797902015955, 6.965998958219364448E-18, -0.01292414190464157182 ) ) ;
#1786 = DIRECTION ( 'NONE',  ( 1.000000000000000000, 0.000000000000000000, 0.000000000000000000 ) ) ;
#1787 = EDGE_LOOP ( 'NONE', ( #18482, #19485 ) ) ;
#1788 = CARTESIAN_POINT ( 'NONE',  ( -91.61331032192597945, 77.62808270880877615, -29.62115891282511271 ) ) ;
#1789 = AXIS2_PLACEMENT_3D ( 'NONE', #20008, #21607, #6011 ) ;
#1790 = ORIENTED_EDGE ( 'NONE', *, *, #20218, .F. ) ;
#1791 = ADVANCED_FACE ( 'NONE', ( #4229 ), #14606, .F. ) ;
#1792 = CYLINDRICAL_SURFACE ( 'NONE', #22008, 6.499999999999998224 ) ;
#1793 = FACE_OUTER_BOUND ( 'NONE', #9967, .T. ) ;
#1794 = ORIENTED_EDGE ( 'NONE', *, *, #18920, .F. ) ;
#1795 = CARTESIAN_POINT ( 'NONE',  ( -8.182603756456146016, 171.4215663745681866, 81.70472014839175756 ) ) ;
#1796 = CARTESIAN_POINT ( 'NONE',  ( 58.84369908111836622, 126.5745674511216947, 103.5878786308435906 ) ) ;
#1797 = ADVANCED_FACE ( 'NONE', ( #11142 ), #18161, .T. ) ;
#1798 = ORIENTED_EDGE ( 'NONE', *, *, #5168, .F. ) ;
#1799 = CARTESIAN_POINT ( 'NONE',  ( -38.21549050681395698, 167.4026153394593734, 273.1339171915171846 ) ) ;
#1800 = ORIENTED_EDGE ( 'NONE', *, *, #21148, .F. ) ;
#1801 = CARTESIAN_POINT ( 'NONE',  ( 2.067862704742617463, 69.99999999999998579, 159.9866367664322979 ) ) ;
#1802 = CIRCLE ( 'NONE', #11336, 22.50000000000000000 ) ;
#1803 = CARTESIAN_POINT ( 'NONE',  ( 50.89197640125190958, 108.0238286078847523, 68.68741454989820738 ) ) ;
#1804 = ORIENTED_EDGE ( 'NONE', *, *, #3211, .F. ) ;
#1805 = CARTESIAN_POINT ( 'NONE',  ( -12.19462927199251112, 185.2216277673267939, 320.4682053348163890 ) ) ;
#1806 = AXIS2_PLACEMENT_3D ( 'NONE', #5627, #7469, #5505 ) ;
#1808 = DIRECTION ( 'NONE',  ( 0.000000000000000000, -1.000000000000000000, 0.000000000000000000 ) ) ;
#1807 = CARTESIAN_POINT ( 'NONE',  ( -38.69757710431294839, 94.02752048664900997, -82.47923521851862461 ) ) ;
#1809 = DIRECTION ( 'NONE',  ( 0.000000000000000000, 0.000000000000000000, 1.000000000000000000 ) ) ;
#1810 = VERTEX_POINT ( 'NONE', #73 ) ;
#1811 = DIRECTION ( 'NONE',  ( -0.7193492748294019190, 0.6946270388778962301, 0.005467875468530753770 ) ) ;
#1812 = CARTESIAN_POINT ( 'NONE',  ( -90.42246537646651916, 78.26562148642790362, 32.93420195958645280 ) ) ;
#1813 = CARTESIAN_POINT ( 'NONE',  ( 15.81758052762976341, 168.0514417711093529, 307.9285322505227782 ) ) ;
#1814 = CARTESIAN_POINT ( 'NONE',  ( -15.16114907798143285, 179.5344160342980615, 315.3037902903944314 ) ) ;
#1815 = VERTEX_POINT ( 'NONE', #7417 ) ;
#1816 = DIRECTION ( 'NONE',  ( 0.01292394549866740169, 0.005513023399720822990, 0.9999012842304693116 ) ) ;
#1817 = ADVANCED_FACE ( 'NONE', ( #5221 ), #10757, .F. ) ;
#1818 = LINE ( 'NONE', #531, #4187 ) ;
#1819 = PRESENTATION_LAYER_ASSIGNMENT (  '', '', ( #11729 ) ) ;
#1820 = LINE ( 'NONE', #8809, #21334 ) ;
#1821 = CARTESIAN_POINT ( 'NONE',  ( 3.872354045398203937, 166.6517708494369856, 299.5967279023338392 ) ) ;
#1822 = ADVANCED_FACE ( 'NONE', ( #192 ), #4319, .F. ) ;
#1823 = CARTESIAN_POINT ( 'NONE',  ( -65.91440269377939387, 103.0000000000000000, -70.32555938675406537 ) ) ;
#1824 = DIRECTION ( 'NONE',  ( 0.9909299940865190504, -0.1338359446631136318, -0.01207007604876911971 ) ) ;
#1825 = CARTESIAN_POINT ( 'NONE',  ( 49.65978088490153652, 110.1615718061116951, -47.45444771764796599 ) ) ;
#1826 = ORIENTED_EDGE ( 'NONE', *, *, #4420, .F. ) ;
#1827 = CARTESIAN_POINT ( 'NONE',  ( 3.600951189929047391, 166.5359973580429482, 278.5988009334944877 ) ) ;
#1828 = LINE ( 'NONE', #5486, #10054 ) ;
#1829 = EDGE_LOOP ( 'NONE', ( #4335, #17107, #8899, #14315, #21275, #17558, #10360, #7844, #3415, #6564 ) ) ;
#1830 = CARTESIAN_POINT ( 'NONE',  ( 49.39923347825703104, 108.3707227317548529, -46.80328957620832142 ) ) ;
#1831 = ORIENTED_EDGE ( 'NONE', *, *, #20609, .T. ) ;
#1832 = LINE ( 'NONE', #20893, #14866 ) ;
#1833 = DIRECTION ( 'NONE',  ( 7.125109674160258889E-05, -0.9999848031710252272, 0.005512562950849896580 ) ) ;
#1834 = CARTESIAN_POINT ( 'NONE',  ( -42.62760890944326775, 168.8862223267045124, 273.1827648312820997 ) ) ;
#1835 = VECTOR ( 'NONE', #19052, 999.9999999999998863 ) ;
#1836 = MANIFOLD_SOLID_BREP ( 'Boss-Extrude1', #868 ) ;
#1837 = ORIENTED_EDGE ( 'NONE', *, *, #5709, .F. ) ;
#1838 = CARTESIAN_POINT ( 'NONE',  ( 4.182528737366220106, 166.7840834110302808, 323.5943587238651276 ) ) ;
#1839 =( NAMED_UNIT ( * ) PLANE_ANGLE_UNIT ( ) SI_UNIT ( $, .RADIAN. ) );
#1840 = CARTESIAN_POINT ( 'NONE',  ( 15.98577074487546312, 168.1231874004433280, 320.9410920942888197 ) ) ;
#1841 = EDGE_CURVE ( 'NONE', #5715, #14396, #16176, .T. ) ;
#1842 = CIRCLE ( 'NONE', #13223, 101.0000000000000000 ) ;
#1843 = CARTESIAN_POINT ( 'NONE',  ( -59.98899403950397158, 118.2576901802692504, 47.66399645013669328 ) ) ;
#1844 = ADVANCED_FACE ( 'NONE', ( #1793 ), #9093, .F. ) ;
#1845 = ORIENTED_EDGE ( 'NONE', *, *, #21487, .T. ) ;
#1846 = DIRECTION ( 'NONE',  ( -0.01292394549866741384, -0.005513023399720269613, -0.9999012842304692006 ) ) ;
#1847 = CARTESIAN_POINT ( 'NONE',  ( -88.16594588878987793, 88.49255433320315944, 52.69555038922003121 ) ) ;
#1848 = CIRCLE ( 'NONE', #19071, 11.00000000000000178 ) ;
#1849 = VERTEX_POINT ( 'NONE', #22654 ) ;
#1850 = AXIS2_PLACEMENT_3D ( 'NONE', #2128, #21419, #5679 ) ;
#1851 = ORIENTED_EDGE ( 'NONE', *, *, #8400, .T. ) ;
#1852 = CARTESIAN_POINT ( 'NONE',  ( 54.52327687265658085, 20.00000000000000000, -111.3697098814019171 ) ) ;
#1853 = VECTOR ( 'NONE', #4021, 1000.000000000000114 ) ;
#1854 = CARTESIAN_POINT ( 'NONE',  ( -34.23497593041177112, 93.68146586044639434, 83.10373569841586061 ) ) ;
#1855 = EDGE_LOOP ( 'NONE', ( #18541, #5060, #3702, #11003 ) ) ;
#1856 = PRODUCT_DEFINITION_FORMATION_WITH_SPECIFIED_SOURCE ( 'ANY', '', #16535, .NOT_KNOWN. ) ;
#1857 = CARTESIAN_POINT ( 'NONE',  ( 84.81034445695703994, 75.01375443481772720, -2.741737533029477092 ) ) ;
#1858 = DIRECTION ( 'NONE',  ( 7.125109674364534776E-05, -0.9999848031710252272, 0.005512562950849704893 ) ) ;
#1859 = ORIENTED_EDGE ( 'NONE', *, *, #7223, .F. ) ;
#1860 = LINE ( 'NONE', #8855, #9890 ) ;
#1861 = AXIS2_PLACEMENT_3D ( 'NONE', #18672, #7651, #20052 ) ;
#1862 = EDGE_LOOP ( 'NONE', ( #12568, #13314, #10724, #19997 ) ) ;
#1863 = DIRECTION ( 'NONE',  ( 0.01292414190464131335, 1.902755938799530239E-22, 0.9999164797902015955 ) ) ;
#1864 = CARTESIAN_POINT ( 'NONE',  ( -10.32533161609876871, 336.9590297039326288, 324.0204083566396207 ) ) ;
#1865 = CARTESIAN_POINT ( 'NONE',  ( -7.642197790895533416, 165.4224147006813155, 321.2648411829814563 ) ) ;
#1866 = ORIENTED_EDGE ( 'NONE', *, *, #21450, .T. ) ;
#1867 = CARTESIAN_POINT ( 'NONE',  ( 39.45263645499988314, 96.15465585523027414, -42.60697859377187058 ) ) ;
#1868 = EDGE_LOOP ( 'NONE', ( #6719, #9572, #17708, #474 ) ) ;
#1869 = DIRECTION ( 'NONE',  ( -0.9999164797902015955, -2.001050586450178695E-22, 0.01292414190464131335 ) ) ;
#1870 =( LENGTH_UNIT ( ) NAMED_UNIT ( * ) SI_UNIT ( .MILLI., .METRE. ) );
#1871 = CIRCLE ( 'NONE', #2959, 1.989999999999997105 ) ;
#1872 = CARTESIAN_POINT ( 'NONE',  ( -50.62696408822809246, 114.2898949143141039, 165.5655560615739148 ) ) ;
#1873 = ORIENTED_EDGE ( 'NONE', *, *, #12470, .F. ) ;
#1874 = PRODUCT_DEFINITION_SHAPE ( 'NONE', 'NONE',  #22688 ) ;
#1875 = VECTOR ( 'NONE', #19004, 1000.000000000000114 ) ;
#1876 = EDGE_CURVE ( 'NONE', #11555, #17908, #8775, .T. ) ;
#1877 = AXIS2_PLACEMENT_3D ( 'NONE', #2545, #11276, #8168 ) ;
#1878 = CARTESIAN_POINT ( 'NONE',  ( -41.41899454747532161, 166.0889136240114681, 277.1829612759436827 ) ) ;
#1879 = VERTEX_POINT ( 'NONE', #21086 ) ;
#1880 = VERTEX_POINT ( 'NONE', #19357 ) ;
#1881 = UNCERTAINTY_MEASURE_WITH_UNIT (LENGTH_MEASURE( 1.000000000000000082E-05 ), #12716, 'distance_accuracy_value', 'NONE');
#1882 = CARTESIAN_POINT ( 'NONE',  ( 15.29545575833136084, 188.7412618571948144, 308.3876529512198204 ) ) ;
#1884 = ORIENTED_EDGE ( 'NONE', *, *, #11653, .T. ) ;
#1883 = ORIENTED_EDGE ( 'NONE', *, *, #18342, .T. ) ;
#1885 = DIRECTION ( 'NONE',  ( 0.01292394549866728373, 0.005513023399720296501, 0.9999012842304693116 ) ) ;
#1886 = DIRECTION ( 'NONE',  ( 0.9999164797902017066, 2.045740421681430110E-15, -0.01292414190464156835 ) ) ;
#1887 = CARTESIAN_POINT ( 'NONE',  ( -8.165269366632555759, 145.2835741796170623, 277.6601055409479386 ) ) ;
#1888 = DIRECTION ( 'NONE',  ( -2.025474946048326158E-22, 1.000000000000000000, -1.876735158486678933E-22 ) ) ;
#1889 = AXIS2_PLACEMENT_3D ( 'NONE', #11521, #2787, #22378 ) ;
#1890 = CARTESIAN_POINT ( 'NONE',  ( -38.70754582269196220, 96.72929363966481731, 84.40869485543453266 ) ) ;
#1891 = B_SPLINE_CURVE_WITH_KNOTS ( 'NONE', 3,
 ( #22507, #7458, #2064, #14497, #21457, #8519, #6800, #13824, #9045, #17390, #20808, #19086, #1647, #3360, #10377, #5178 ),
 .UNSPECIFIED., .F., .F.,
 ( 4, 2, 2, 2, 2, 2, 2, 4 ),
 ( -3.123367963899254272E-05, 0.001725203944011495299, 0.003481641567661983121, 0.006994516814962895880, 0.008750954438613373076, 0.01050739206226384941, 0.01226382968591432573, 0.01402026730956480380 ),
 .UNSPECIFIED. ) ;
#1892 = PRODUCT_DEFINITION_SHAPE ( 'NONE', 'NONE',  #18443 ) ;
#1893 = CARTESIAN_POINT ( 'NONE',  ( 13.03751462902003055, 190.3043364584464143, 320.8506857707324684 ) ) ;
#1894 = CARTESIAN_POINT ( 'NONE',  ( 77.90572232234517003, 75.18523895546071856, -6.939197329751477739 ) ) ;
#1895 = VECTOR ( 'NONE', #20236, 999.9999999999998863 ) ;
#1896 = CARTESIAN_POINT ( 'NONE',  ( 16.47746874666049166, 185.3946093038764218, 306.5053848239848548 ) ) ;
#1897 = CARTESIAN_POINT ( 'NONE',  ( 84.57230515545197136, 105.0000000000000000, 70.33944174062776256 ) ) ;
#1898 = CARTESIAN_POINT ( 'NONE',  ( 1.364374644014609697E-14, 69.99999999999998579, -9.836443712999143722E-15 ) ) ;
#1899 = EDGE_LOOP ( 'NONE', ( #5563, #2921, #4892, #3591 ) ) ;
#1900 = AXIS2_PLACEMENT_3D ( 'NONE', #17981, #5764, #738 ) ;
#1901 = EDGE_CURVE ( 'NONE', #4209, #1243, #18281, .T. ) ;
#1902 = CARTESIAN_POINT ( 'NONE',  ( -9.012827358357725416, 186.4798162552521603, 321.5937060577796842 ) ) ;
#1903 = CARTESIAN_POINT ( 'NONE',  ( 13.28235005706528682, 159.1720975239875884, 299.5163413053770682 ) ) ;
#1904 = VERTEX_POINT ( 'NONE', #21306 ) ;
#1906 = CARTESIAN_POINT ( 'NONE',  ( -92.11236706770199589, 79.08401524093159196, -26.36688770261625336 ) ) ;
#1905 = AXIS2_PLACEMENT_3D ( 'NONE', #16224, #921, #17933 ) ;
#1907 = ADVANCED_FACE ( 'NONE', ( #3621 ), #22276, .F. ) ;
#1908 = ORIENTED_EDGE ( 'NONE', *, *, #12235, .T. ) ;
#1909 = AXIS2_PLACEMENT_3D ( 'NONE', #9756, #18257, #14830 ) ;
#1910 = EDGE_CURVE ( 'NONE', #1979, #4369, #21194, .T. ) ;
#1911 = AXIS2_PLACEMENT_3D ( 'NONE', #7697, #5853, #21910 ) ;
#1912 = CARTESIAN_POINT ( 'NONE',  ( 1.117803423002110774, 45.00000000000000000, 109.6947150755565161 ) ) ;
#1913 = CIRCLE ( 'NONE', #12565, 75.00000000000002842 ) ;
#1914 = FILL_AREA_STYLE_COLOUR ( '', #15733 ) ;
#1915 = MANIFOLD_SOLID_BREP ( 'Stock-MAS-425-1', #16147 ) ;
#1916 = APPLICATION_CONTEXT ( 'automotive_design' ) ;
#1917 = EDGE_CURVE ( 'NONE', #5531, #19256, #2593, .T. ) ;
#1918 = DIRECTION ( 'NONE',  ( 7.125109674160325297E-05, -0.9999848031710253382, 0.005512562950849327591 ) ) ;
#1919 = ORIENTED_EDGE ( 'NONE', *, *, #14078, .T. ) ;
#1920 = EDGE_CURVE ( 'NONE', #12267, #12564, #7508, .T. ) ;
#1921 = CARTESIAN_POINT ( 'NONE',  ( 12.33097383755215937, 187.6544282282688414, 322.9682109676994628 ) ) ;
#1922 = DIRECTION ( 'NONE',  ( 0.01292414190463830014, 0.000000000000000000, 0.9999164797902017066 ) ) ;
#1923 = AXIS2_PLACEMENT_3D ( 'NONE', #18598, #18929, #6322 ) ;
#1924 = CONICAL_SURFACE ( 'NONE', #13673, 3.309500000000002107, 0.7853981633974710386 ) ;
#1925 = EDGE_CURVE ( 'NONE', #15977, #18898, #7876, .T. ) ;
#1926 = CARTESIAN_POINT ( 'NONE',  ( -157.5176307659779127, 20.00000000000000000, 60.94675664190624786 ) ) ;
#1927 = CARTESIAN_POINT ( 'NONE',  ( -9.866459160504181369, 187.6519449355448046, 321.1574017861566972 ) ) ;
#1928 = DIRECTION ( 'NONE',  ( 7.125109674403276030E-05, -0.9999848031710252272, 0.005512562950848280685 ) ) ;
#1929 = FACE_BOUND ( 'NONE', #434, .T. ) ;
#1930 = VERTEX_POINT ( 'NONE', #16741 ) ;
#1931 = CARTESIAN_POINT ( 'NONE',  ( -15.16562817910661387, 179.5584899311543552, 314.0881026776677345 ) ) ;
#1932 = FACE_OUTER_BOUND ( 'NONE', #2191, .T. ) ;
#1933 = VECTOR ( 'NONE', #14856, 1000.000000000000000 ) ;
#1934 = CARTESIAN_POINT ( 'NONE',  ( -5.731715098087012628, 326.6288426432528240, 307.3396573775339107 ) ) ;
#1935 = CARTESIAN_POINT ( 'NONE',  ( -13.94857819362903939, 180.2051281715647804, 318.6524844431677934 ) ) ;
#1936 = ADVANCED_FACE ( 'NONE', ( #536 ), #9602, .T. ) ;
#1937 = CARTESIAN_POINT ( 'NONE',  ( 19.54762674317498039, 182.9836852283762880, 309.9251239444264456 ) ) ;
#1938 = EDGE_CURVE ( 'NONE', #19786, #13316, #13517, .T. ) ;
#1939 = ORIENTED_EDGE ( 'NONE', *, *, #11044, .T. ) ;
#1940 = CIRCLE ( 'NONE', #12591, 77.00000000000002842 ) ;
#1941 = AXIS2_PLACEMENT_3D ( 'NONE', #12342, #16027, #14182 ) ;
#1942 = CARTESIAN_POINT ( 'NONE',  ( -10.14484841738276089, 81.92452521006620714, -88.15032624680998197 ) ) ;
#1943 = ORIENTED_EDGE ( 'NONE', *, *, #18930, .F. ) ;
#1944 = PLANE ( 'NONE',  #2313 ) ;
#1945 = PLANE ( 'NONE',  #14360 ) ;
#1946 = DIRECTION ( 'NONE',  ( -2.459148776294495979E-24, 1.000000000000000000, -1.902597020224326827E-22 ) ) ;
#1947 = CLOSED_SHELL ( 'NONE', ( #12781, #6146, #12871, #3592, #4295, #12353, #17971, #17861, #11488, #11202, #3726, #7553, #6285, #13146, #19336, #8004, #12457, #13217, #3035, #16807, #11624, #2048, #17096, #16134, #7945, #20890, #15996, #16001 ) ) ;
#1948 = EDGE_CURVE ( 'NONE', #20716, #899, #20793, .T. ) ;
#1949 = DIRECTION ( 'NONE',  ( 0.009760756503427813965, -0.9999378516499565217, 0.005387065077607405654 ) ) ;
#1950 = CYLINDRICAL_SURFACE ( 'NONE', #17036, 2.499999999999988010 ) ;
#1951 = EDGE_LOOP ( 'NONE', ( #2676, #18595, #18575, #10980 ) ) ;
#1952 = EDGE_CURVE ( 'NONE', #18558, #11233, #1042, .T. ) ;
#1953 = CARTESIAN_POINT ( 'NONE',  ( -48.85087316658617596, 95.00692584804919250, -43.47488344668517612 ) ) ;
#1954 = ORIENTED_EDGE ( 'NONE', *, *, #17504, .T. ) ;
#1956 = DIRECTION ( 'NONE',  ( -0.01292394549866743465, -0.005513023399721021615, -0.9999012842304692006 ) ) ;
#1955 = CARTESIAN_POINT ( 'NONE',  ( 106.3959516824313596, 78.65697569891375451, 27.92701496092258040 ) ) ;
#1957 = DIRECTION ( 'NONE',  ( 0.000000000000000000, 0.000000000000000000, -1.000000000000000000 ) ) ;
#1958 = CARTESIAN_POINT ( 'NONE',  ( 39.11273342774209283, 91.99797716581187501, 83.46418088055293083 ) ) ;
#1959 = CIRCLE ( 'NONE', #13704, 10.00000000000005684 ) ;
#1960 = MANIFOLD_SOLID_BREP ( 'Stock-MAS-425-1', #5092 ) ;
#1961 = AXIS2_PLACEMENT_3D ( 'NONE', #5271, #6777, #12316 ) ;
#1962 = EDGE_LOOP ( 'NONE', ( #14254, #780, #7957, #4938 ) ) ;
#1963 = CARTESIAN_POINT ( 'NONE',  ( 85.01653497985981289, 104.3814432989690602, -69.80106575130697877 ) ) ;
#1964 = CARTESIAN_POINT ( 'NONE',  ( 36.36981073755603688, 93.68077716319862702, 82.19051635825725555 ) ) ;
#1965 = CARTESIAN_POINT ( 'NONE',  ( 18.46443518240318937, 168.4037924862991815, 320.2340148651496179 ) ) ;
#1966 = EDGE_CURVE ( 'NONE', #9119, #13016, #18107, .T. ) ;
#1967 = VERTEX_POINT ( 'NONE', #6596 ) ;
#1968 = AXIS2_PLACEMENT_3D ( 'NONE', #15363, #22311, #17298 ) ;
#1969 = DIRECTION ( 'NONE',  ( -0.000000000000000000, -1.000000000000000000, -0.000000000000000000 ) ) ;
#1970 = CARTESIAN_POINT ( 'NONE',  ( -88.16914282057626906, 88.71763460176525484, 52.39312110959539837 ) ) ;
#1971 = CIRCLE ( 'NONE', #19570, 10.00000000000001599 ) ;
#1972 = ORIENTED_EDGE ( 'NONE', *, *, #18630, .F. ) ;
#1973 = TOROIDAL_SURFACE ( 'NONE', #20288, 77.00000000000002842, 2.000000000000000000 ) ;
#1974 = ORIENTED_EDGE ( 'NONE', *, *, #19587, .T. ) ;
#1975 = FACE_OUTER_BOUND ( 'NONE', #9307, .T. ) ;
#1976 = DIRECTION ( 'NONE',  ( 0.01292394549866728200, 0.005513023399720295634, 0.9999012842304692006 ) ) ;
#1977 = CARTESIAN_POINT ( 'NONE',  ( 80.39208672325557359, 75.13699351169599083, 4.061340467186282943 ) ) ;
#1978 = DIRECTION ( 'NONE',  ( -0.000000000000000000, -0.000000000000000000, 1.000000000000000000 ) ) ;
#1979 = VERTEX_POINT ( 'NONE', #8220 ) ;
#1980 = ADVANCED_FACE ( 'NONE', ( #20604 ), #15249, .T. ) ;
#1981 = CARTESIAN_POINT ( 'NONE',  ( 91.23296681615025250, 78.26422321607692822, 30.58575029229923459 ) ) ;
#1982 = ORIENTED_EDGE ( 'NONE', *, *, #1431, .F. ) ;
#1983 = DIRECTION ( 'NONE',  ( 0.01292394549866738955, 0.005513023399720468239, 0.9999012842304693116 ) ) ;
#1984 = EDGE_CURVE ( 'NONE', #14056, #15010, #6897, .T. ) ;
#1985 = DIRECTION ( 'NONE',  ( -0.01292394549866738782, -0.005513023399720700692, -0.9999012842304693116 ) ) ;
#1986 = CIRCLE ( 'NONE', #14841, 3.399999999999992806 ) ;
#1987 = CARTESIAN_POINT ( 'NONE',  ( 13.59252474903330210, 159.3044100855808836, 323.5139721269083566 ) ) ;
#1988 = CARTESIAN_POINT ( 'NONE',  ( -12.65694952506544801, 164.8377797042643635, 318.5015202093982225 ) ) ;
#1989 = VERTEX_POINT ( 'NONE', #11897 ) ;
#1990 = CARTESIAN_POINT ( 'NONE',  ( 40.57369421770351892, 106.0982379271226677, 198.8762978010233553 ) ) ;
#1991 = VERTEX_POINT ( 'NONE', #18883 ) ;
#1992 = LINE ( 'NONE', #156, #21366 ) ;
#1993 = SURFACE_STYLE_USAGE ( .BOTH. , #12447 ) ;
#1994 = CIRCLE ( 'NONE', #17413, 2.999999999999988898 ) ;
#1995 = DIRECTION ( 'NONE',  ( -0.9999164797902017066, -2.001050586450178931E-22, 0.01292414190464131508 ) ) ;
#1996 = ORIENTED_EDGE ( 'NONE', *, *, #8299, .F. ) ;
#1997 = VECTOR ( 'NONE', #15627, 1000.000000000000000 ) ;
#1998 = PLANE ( 'NONE',  #3714 ) ;
#1999 = VERTEX_POINT ( 'NONE', #17170 ) ;
#2000 = EDGE_LOOP ( 'NONE', ( #18719, #17410, #7375, #11157 ) ) ;
#2001 = ORIENTED_EDGE ( 'NONE', *, *, #7053, .F. ) ;
#2002 = DIRECTION ( 'NONE',  ( -0.01035335185279151644, -0.005513005182356664133, -0.9999312050732649393 ) ) ;
#2003 = AXIS2_PLACEMENT_3D ( 'NONE', #9292, #4227, #460 ) ;
#2004 = ORIENTED_EDGE ( 'NONE', *, *, #13878, .T. ) ;
#2005 = DIRECTION ( 'NONE',  ( -0.8504393858994485633, 0.002839416958724588855, 0.5260653843604455870 ) ) ;
#2006 = CARTESIAN_POINT ( 'NONE',  ( 41.42670316190684332, 94.99786382055523859, -44.62631324292065926 ) ) ;
#2007 = DIRECTION ( 'NONE',  ( 0.6979091139780386754, -0.003898296230784643879, -0.7161757269782926816 ) ) ;
#2008 = AXIS2_PLACEMENT_3D ( 'NONE', #10847, #16145, #21169 ) ;
#2009 = CARTESIAN_POINT ( 'NONE',  ( -64.28883878761490678, 83.29019440189556178, 55.44125366118054643 ) ) ;
#2010 = CARTESIAN_POINT ( 'NONE',  ( -40.52114077660952773, 94.71095003552228775, 83.69340898796828299 ) ) ;
#2011 = ADVANCED_FACE ( 'NONE', ( #1442 ), #8422, .T. ) ;
#2012 = DIRECTION ( 'NONE',  ( -0.9934404589540163366, -0.1135548637187053511, 0.01346653032743023309 ) ) ;
#2013 = CARTESIAN_POINT ( 'NONE',  ( 18.63884989169994100, 183.8434042675073954, 310.4714192387435787 ) ) ;
#2014 = CARTESIAN_POINT ( 'NONE',  ( 91.26841073957255901, 80.27011201451718136, 30.02500290034332053 ) ) ;
#2015 = CARTESIAN_POINT ( 'NONE',  ( 89.40819020483024815, 79.89452498912716294, 28.94780723987645388 ) ) ;
#2016 = ORIENTED_EDGE ( 'NONE', *, *, #19731, .F. ) ;
#2017 = VECTOR ( 'NONE', #16254, 1000.000000000000114 ) ;
#2018 = CARTESIAN_POINT ( 'NONE',  ( 64.99457118636311748, 177.0000000000003695, -0.8400692238016915780 ) ) ;
#2019 = DIRECTION ( 'NONE',  ( -0.01292394549866731669, -0.005513023399720593139, -0.9999012842304692006 ) ) ;
#2020 = ORIENTED_EDGE ( 'NONE', *, *, #235, .T. ) ;
#2021 = CARTESIAN_POINT ( 'NONE',  ( -92.18978923775263468, 77.29775901949990669, -29.08785173819802594 ) ) ;
#2022 = ORIENTED_EDGE ( 'NONE', *, *, #9067, .T. ) ;
#2023 = EDGE_LOOP ( 'NONE', ( #2142, #11774, #15367, #15903 ) ) ;
#2024 = CARTESIAN_POINT ( 'NONE',  ( -3.200698602031742723, 70.00000000000000000, -81.18156990192605349 ) ) ;
#2025 = DIRECTION ( 'NONE',  ( 0.01292394549866743812, 0.005513023399720639109, 0.9999012842304693116 ) ) ;
#2026 = MECHANICAL_DESIGN_GEOMETRIC_PRESENTATION_REPRESENTATION (  '', ( #3118 ), #7538 ) ;
#2027 = ORIENTED_EDGE ( 'NONE', *, *, #6679, .F. ) ;
#2028 = DIRECTION ( 'NONE',  ( 0.000000000000000000, 0.000000000000000000, -1.000000000000000000 ) ) ;
#2029 = DIRECTION ( 'NONE',  ( -2.025474946048326158E-22, 1.000000000000000000, -1.876735158486678933E-22 ) ) ;
#2030 = ORIENTED_EDGE ( 'NONE', *, *, #6944, .T. ) ;
#2031 = CARTESIAN_POINT ( 'NONE',  ( 12.21332820092900739, 188.3547093575519682, 320.9587726345017131 ) ) ;
#2032 = ORIENTED_EDGE ( 'NONE', *, *, #8503, .F. ) ;
#2033 = CARTESIAN_POINT ( 'NONE',  ( 45.23703820192896075, 164.1026264709443865, 18.04839321081418291 ) ) ;
#2034 = ADVANCED_FACE ( 'NONE', ( #4971 ), #12001, .T. ) ;
#2035 = CARTESIAN_POINT ( 'NONE',  ( 71.51920288841776596, 92.50622980579329635, 83.57642618781942190 ) ) ;
#2036 = FILL_AREA_STYLE_COLOUR ( '', #13310 ) ;
#2038 = CARTESIAN_POINT ( 'NONE',  ( -55.34026779967800280, 145.4210017871401703, 167.4659909391495773 ) ) ;
#2037 = CARTESIAN_POINT ( 'NONE',  ( -92.27487665212996149, 79.82259189700857860, 31.19759217298344822 ) ) ;
#2039 = CARTESIAN_POINT ( 'NONE',  ( 396.0414077195426898, 177.0000000000003695, -5.118922886994747401 ) ) ;
#2040 = ORIENTED_EDGE ( 'NONE', *, *, #14453, .T. ) ;
#2041 = CARTESIAN_POINT ( 'NONE',  ( -14.34866974388063099, 181.6106202444769906, 311.1517963829039104 ) ) ;
#2042 = DIRECTION ( 'NONE',  ( -0.01292394549866741384, -0.005513023399720269613, -0.9999012842304692006 ) ) ;
#2043 = DIRECTION ( 'NONE',  ( -7.125109674243555432E-05, 0.9999848031710253382, -0.005512562950850175003 ) ) ;
#2044 = CARTESIAN_POINT ( 'NONE',  ( -15.06566084134985850, 178.6016716131798887, 315.4181938385037256 ) ) ;
#2045 = VECTOR ( 'NONE', #16778, 1000.000000000000227 ) ;
#2046 = CARTESIAN_POINT ( 'NONE',  ( -16.82962413914983912, 177.4987173824078468, 90.66609475777795524 ) ) ;
#2047 = EDGE_CURVE ( 'NONE', #22611, #2091, #8370, .T. ) ;
#2048 = ADVANCED_FACE ( 'NONE', ( #19222 ), #3710, .T. ) ;
#2049 = DIRECTION ( 'NONE',  ( 0.01292414190464131335, 1.902755938799530239E-22, 0.9999164797902015955 ) ) ;
#2050 = EDGE_CURVE ( 'NONE', #7916, #1999, #12117, .T. ) ;
#2051 = FACE_OUTER_BOUND ( 'NONE', #14958, .T. ) ;
#2052 = DIRECTION ( 'NONE',  ( 7.125109674364536131E-05, -0.9999848031710253382, 0.005512562950849705760 ) ) ;
#2053 = FACE_OUTER_BOUND ( 'NONE', #8199, .T. ) ;
#2054 = ORIENTED_EDGE ( 'NONE', *, *, #3429, .T. ) ;
#2055 = AXIS2_PLACEMENT_3D ( 'NONE', #10342, #14142, #5029 ) ;
#2056 = EDGE_CURVE ( 'NONE', #12292, #4350, #1669, .T. ) ;
#2057 = ORIENTED_EDGE ( 'NONE', *, *, #3919, .F. ) ;
#2058 = CARTESIAN_POINT ( 'NONE',  ( -4.905708827035327069, 164.7686025659857023, 81.69904712205610053 ) ) ;
#2059 = DIRECTION ( 'NONE',  ( -0.01292394549866632963, -0.005513023399716958026, -0.9999012842304692006 ) ) ;
#2060 = VERTEX_POINT ( 'NONE', #14306 ) ;
#2061 = EDGE_CURVE ( 'NONE', #10705, #9211, #22294, .T. ) ;
#2062 = CARTESIAN_POINT ( 'NONE',  ( 39.42082737383937996, 72.00000000000000000, -83.51645567887783272 ) ) ;
#2063 = ORIENTED_EDGE ( 'NONE', *, *, #17873, .T. ) ;
#2064 = CARTESIAN_POINT ( 'NONE',  ( -3.133037003347189042, 189.9394842237717569, 275.0803702628431893 ) ) ;
#2065 =( LENGTH_UNIT ( ) NAMED_UNIT ( * ) SI_UNIT ( .MILLI., .METRE. ) );
#2066 = CARTESIAN_POINT ( 'NONE',  ( -1.163172771417702700, 30.00000000000000711, -89.99248318111824574 ) ) ;
#2067 = CARTESIAN_POINT ( 'NONE',  ( -50.59154831888564274, 96.21415597129798414, -45.44386052779758245 ) ) ;
#2068 = CARTESIAN_POINT ( 'NONE',  ( -55.90530736925617816, 114.7828611649933350, 163.2967483362970427 ) ) ;
#2069 = EDGE_CURVE ( 'NONE', #21740, #9403, #15804, .T. ) ;
#2070 = VERTEX_POINT ( 'NONE', #16151 ) ;
#2071 = EDGE_LOOP ( 'NONE', ( #21343, #20643, #4649 ) ) ;
#2072 = CARTESIAN_POINT ( 'NONE',  ( 14.28162271022098295, 144.6901722051186994, 276.8194863368150891 ) ) ;
#2073 =( BOUNDED_CURVE ( )  B_SPLINE_CURVE ( 3, ( #15853, #13880, #22563, #20867 ),
 .UNSPECIFIED., .F., .T. ) 
 B_SPLINE_CURVE_WITH_KNOTS ( ( 4, 4 ),
 ( 5.433035758877964305, 5.587168164874065646 ),
 .UNSPECIFIED. ) 
 CURVE ( )  GEOMETRIC_REPRESENTATION_ITEM ( )  RATIONAL_B_SPLINE_CURVE ( ( 1.000000000000000000, 0.9980212464270939998, 0.9980212464270939998, 1.000000000000000000 ) ) 
 REPRESENTATION_ITEM ( '' )  );
#2074 = LINE ( 'NONE', #19406, #9156 ) ;
#2075 = ADVANCED_FACE ( 'NONE', ( #17761 ), #10508, .F. ) ;
#2076 = CARTESIAN_POINT ( 'NONE',  ( 19.65277869176573233, 186.5675413641987461, 276.1968354304440254 ) ) ;
#2077 = ORIENTED_EDGE ( 'NONE', *, *, #16606, .T. ) ;
#2078 = DIRECTION ( 'NONE',  ( -0.01292414190464044946, -1.902755938799528593E-22, -0.9999164797902015955 ) ) ;
#2079 = CARTESIAN_POINT ( 'NONE',  ( -88.16613847108702373, 88.50822752828271689, 52.67809515463711989 ) ) ;
#2080 = EDGE_CURVE ( 'NONE', #18285, #6117, #7049, .T. ) ;
#2081 = PRODUCT_CONTEXT ( 'NONE', #15292, 'mechanical' ) ;
#2082 = ORIENTED_EDGE ( 'NONE', *, *, #20790, .F. ) ;
#2083 = EDGE_LOOP ( 'NONE', ( #11750, #18115, #4859, #7474 ) ) ;
#2084 = DIRECTION ( 'NONE',  ( 0.01292414190464131508, 0.000000000000000000, 0.9999164797902017066 ) ) ;
#2085 = CARTESIAN_POINT ( 'NONE',  ( 88.40906079701872500, 78.43035437438885538, -33.14537955645114664 ) ) ;
#2086 = DIRECTION ( 'NONE',  ( 0.01035335185279032469, 0.005513005182356926943, 0.9999312050732648283 ) ) ;
#2087 = DIRECTION ( 'NONE',  ( -0.9999164797902015955, -2.001050586450180341E-22, 0.01292414190464038874 ) ) ;
#2088 = VERTEX_POINT ( 'NONE', #22628 ) ;
#2089 = ADVANCED_FACE ( 'NONE', ( #12577 ), #8646, .F. ) ;
#2090 = CARTESIAN_POINT ( 'NONE',  ( 92.50752184771765485, 77.20349362929610493, 28.92971669647237576 ) ) ;
#2091 = VERTEX_POINT ( 'NONE', #6924 ) ;
#2092 = FACE_BOUND ( 'NONE', #12857, .T. ) ;
#2093 = CARTESIAN_POINT ( 'NONE',  ( 65.34011313256004883, 145.1470193978928478, 25.89385934263130196 ) ) ;
#2094 = CARTESIAN_POINT ( 'NONE',  ( -75.60071948563958699, 75.03398072390713480, -1.579025930907502318 ) ) ;
#2095 = CARTESIAN_POINT ( 'NONE',  ( -26.01799913968005384, 324.3151495388358967, 308.8842677255468061 ) ) ;
#2096 = DIRECTION ( 'NONE',  ( 0.000000000000000000, 0.000000000000000000, 1.000000000000000000 ) ) ;
#2097 = FACE_OUTER_BOUND ( 'NONE', #4084, .T. ) ;
#2098 = DIRECTION ( 'NONE',  ( -0.9934404589540177799, -0.1135548637186921672, 0.01346653032743275538 ) ) ;
#2099 = CARTESIAN_POINT ( 'NONE',  ( -10.95260071218788767, 105.6586476617446380, 119.8001432315898001 ) ) ;
#2100 = EDGE_LOOP ( 'NONE', ( #20940, #11395, #17245, #7655, #16464, #6898, #6647, #17037, #21021, #783, #13454, #13565, #12886, #17622 ) ) ;
#2101 = LINE ( 'NONE', #1660, #12535 ) ;
#2102 = ORIENTED_EDGE ( 'NONE', *, *, #6323, .T. ) ;
#2103 = ORIENTED_EDGE ( 'NONE', *, *, #18624, .T. ) ;
#2104 = CARTESIAN_POINT ( 'NONE',  ( -41.56623493000981284, 91.17157287525390075, -82.46967996629571473 ) ) ;
#2105 = EDGE_CURVE ( 'NONE', #3748, #11233, #10394, .T. ) ;
#2106 = ORIENTED_EDGE ( 'NONE', *, *, #19715, .T. ) ;
#2107 = VECTOR ( 'NONE', #22509, 1000.000000000000000 ) ;
#2108 = DIRECTION ( 'NONE',  ( 0.9999164797902015955, 2.001050586450177050E-22, -0.01292414190464223796 ) ) ;
#2109 = CARTESIAN_POINT ( 'NONE',  ( -44.31114033011734676, 178.1114032988642748, 275.1538586390841488 ) ) ;
#2110 = DIRECTION ( 'NONE',  ( -5.440186201345738641E-18, -1.000000000000000000, -1.334940939666364181E-17 ) ) ;
#2111 = PLANE ( 'NONE',  #9688 ) ;
#2112 = CARTESIAN_POINT ( 'NONE',  ( -39.92320284967681232, 94.09382044627800212, 84.30970454134384795 ) ) ;
#2113 = ADVANCED_FACE ( 'NONE', ( #17521 ), #17632, .T. ) ;
#2114 = CARTESIAN_POINT ( 'NONE',  ( 74.53966632203987785, 75.05140447157583594, -4.093706810995048961 ) ) ;
#2115 = CARTESIAN_POINT ( 'NONE',  ( 13.58411996604009886, 190.0215289310135347, 307.9295376775164073 ) ) ;
#2116 = DIRECTION ( 'NONE',  ( 0.9999164797902015955, 2.001050586498092550E-22, -0.01292414190464117457 ) ) ;
#2117 = CARTESIAN_POINT ( 'NONE',  ( 91.38403781951994631, 79.16811561863680424, 26.65243986599108794 ) ) ;
#2118 = EDGE_LOOP ( 'NONE', ( #1686, #12689, #13822, #81 ) ) ;
#2119 = CIRCLE ( 'NONE', #14983, 4.999999999999990230 ) ;
#2120 = LINE ( 'NONE', #3729, #11025 ) ;
#2121 = CARTESIAN_POINT ( 'NONE',  ( -10.85980368455889433, 163.6991139211620236, 126.9796742121690443 ) ) ;
#2122 = ORIENTED_EDGE ( 'NONE', *, *, #8358, .T. ) ;
#2123 = DIRECTION ( 'NONE',  ( -0.01292394549866695240, -0.005513023399725255208, -0.9999012842304693116 ) ) ;
#2124 = ORIENTED_EDGE ( 'NONE', *, *, #20018, .T. ) ;
#2125 = EDGE_CURVE ( 'NONE', #14118, #1904, #9858, .T. ) ;
#2126 = EDGE_CURVE ( 'NONE', #5284, #19030, #14428, .T. ) ;
#2127 = AXIS2_PLACEMENT_3D ( 'NONE', #22218, #2941, #10413 ) ;
#2128 = CARTESIAN_POINT ( 'NONE',  ( -41.52755568966412625, 166.0426042274538077, 268.7837904884077034 ) ) ;
#2129 = SURFACE_STYLE_USAGE ( .BOTH. , #7189 ) ;
#2130 = CARTESIAN_POINT ( 'NONE',  ( 146.5000000000000000, 20.00000000000000000, -2.025191382850354537E-12 ) ) ;
#2131 = MECHANICAL_DESIGN_GEOMETRIC_PRESENTATION_REPRESENTATION (  '', ( #12042 ), #13530 ) ;
#2132 = ORIENTED_EDGE ( 'NONE', *, *, #423, .T. ) ;
#2133 = CARTESIAN_POINT ( 'NONE',  ( 12.23821171205838709, 188.3449730651813638, 320.9566317594674274 ) ) ;
#2134 = VERTEX_POINT ( 'NONE', #8879 ) ;
#2135 = ORIENTED_EDGE ( 'NONE', *, *, #5396, .T. ) ;
#2136 = LINE ( 'NONE', #12384, #22139 ) ;
#2137 = PRODUCT_DEFINITION ( 'UNKNOWN', '', #8434, #18911 ) ;
#2138 = CARTESIAN_POINT ( 'NONE',  ( 67.13053572995309537, 70.13637825286164684, -87.14080137989780894 ) ) ;
#2139 = CARTESIAN_POINT ( 'NONE',  ( -9.651817171046198851, 185.0982321658034948, 321.2476234092152367 ) ) ;
#2140 = CARTESIAN_POINT ( 'NONE',  ( -14.37471740060550118, 109.6998846769365628, 127.3137863664913425 ) ) ;
#2141 = CARTESIAN_POINT ( 'NONE',  ( -80.05923150692979107, 54.99999999999999289, -4.065642694558677661 ) ) ;
#2142 = ORIENTED_EDGE ( 'NONE', *, *, #6607, .T. ) ;
#2143 = AXIS2_PLACEMENT_3D ( 'NONE', #20458, #20572, #8295 ) ;
#2144 = CARTESIAN_POINT ( 'NONE',  ( -15.18631308743390740, 179.4818830208618010, 314.7524899164025101 ) ) ;
#2145 = ORIENTED_EDGE ( 'NONE', *, *, #4888, .F. ) ;
#2146 = CARTESIAN_POINT ( 'NONE',  ( 45.23671757199362986, 168.6025580852140138, 18.02358667753535926 ) ) ;
#2147 = CARTESIAN_POINT ( 'NONE',  ( -10.85595612533484911, 109.6999345499266525, 127.2773526115149281 ) ) ;
#2148 = CARTESIAN_POINT ( 'NONE',  ( -14.75085724879592419, 179.0757283420780936, 316.9950527168435883 ) ) ;
#2149 = ORIENTED_EDGE ( 'NONE', *, *, #18426, .T. ) ;
#2150 = VERTEX_POINT ( 'NONE', #15925 ) ;
#2151 = ADVANCED_FACE ( 'NONE', ( #276 ), #5544, .T. ) ;
#2152 = DIRECTION ( 'NONE',  ( -0.9934404589540165587, -0.1135548637187044907, 0.01346653032743213955 ) ) ;
#2153 = ORIENTED_EDGE ( 'NONE', *, *, #21573, .T. ) ;
#2154 = DIRECTION ( 'NONE',  ( -2.025474946048326158E-22, 1.000000000000000000, -1.876735158486678933E-22 ) ) ;
#2155 = CONTEXT_DEPENDENT_SHAPE_REPRESENTATION ( #21719, #13792 ) ;
#2156 = AXIS2_PLACEMENT_3D ( 'NONE', #8737, #13938, #14184 ) ;
#2157 = DIRECTION ( 'NONE',  ( -7.125109674403837105E-05, 0.9999848031710252272, -0.005512562950847867821 ) ) ;
#2158 = CARTESIAN_POINT ( 'NONE',  ( 41.19638261157624015, 121.2962013336460814, 247.0525242307099347 ) ) ;
#2159 = AXIS2_PLACEMENT_3D ( 'NONE', #8263, #9869, #18495 ) ;
#2160 = CARTESIAN_POINT ( 'NONE',  ( -1.163172771417702700, 69.99999999999998579, -89.99248318111824574 ) ) ;
#2161 = EDGE_LOOP ( 'NONE', ( #15991, #9452, #19555, #18830 ) ) ;
#2162 = ORIENTED_EDGE ( 'NONE', *, *, #16280, .T. ) ;
#2163 = CYLINDRICAL_SURFACE ( 'NONE', #1381, 1.999999999999998446 ) ;
#2164 = CARTESIAN_POINT ( 'NONE',  ( -50.21426504490502651, 95.50261743988794194, -44.28974071693060210 ) ) ;
#2165 = ORIENTED_EDGE ( 'NONE', *, *, #12912, .F. ) ;
#2166 = DIRECTION ( 'NONE',  ( 0.9999164797902015955, 6.965998958219364448E-18, -0.01292414190464157182 ) ) ;
#2167 = DIRECTION ( 'NONE',  ( 0.9999164797902015955, 6.965998958219364448E-18, -0.01292414190464157182 ) ) ;
#2168 = DIRECTION ( 'NONE',  ( 0.000000000000000000, 1.000000000000000000, -0.000000000000000000 ) ) ;
#2169 = CARTESIAN_POINT ( 'NONE',  ( 4.092765588129412713, 86.14799269895429745, 74.95397050060127242 ) ) ;
#2170 = VERTEX_POINT ( 'NONE', #14650 ) ;
#2171 = CARTESIAN_POINT ( 'NONE',  ( -39.99665919160808869, 170.0000000000000284, 0.5169656761856410432 ) ) ;
#2172 = CLOSED_SHELL ( 'NONE', ( #244, #3472, #21006, #18530, #524, #2901, #10105, #7806 ) ) ;
#2173 = CIRCLE ( 'NONE', #20872, 5.999999999999999112 ) ;
#2174 = CARTESIAN_POINT ( 'NONE',  ( -3.467698610696717143, 81.64298031427459534, -99.36756502071499142 ) ) ;
#2175 = VECTOR ( 'NONE', #10101, 1000.000000000000000 ) ;
#2176 = ORIENTED_EDGE ( 'NONE', *, *, #10086, .F. ) ;
#2177 = EDGE_CURVE ( 'NONE', #4506, #8789, #15389, .T. ) ;
#2178 = CARTESIAN_POINT ( 'NONE',  ( -10.85572812182527613, 106.4999831797793775, 127.2949928129576733 ) ) ;
#2179 = EDGE_CURVE ( 'NONE', #15481, #22379, #18418, .T. ) ;
#2180 = PRODUCT_CONTEXT ( 'NONE', #2212, 'mechanical' ) ;
#2182 = ORIENTED_EDGE ( 'NONE', *, *, #8536, .T. ) ;
#2181 = EDGE_LOOP ( 'NONE', ( #3410, #6188, #11314, #6338 ) ) ;
#2183 = ORIENTED_EDGE ( 'NONE', *, *, #15429, .F. ) ;
#2184 = LINE ( 'NONE', #21035, #3366 ) ;
#2185 = DIRECTION ( 'NONE',  ( -0.000000000000000000, -1.000000000000000000, -0.000000000000000000 ) ) ;
#2186 = TOROIDAL_SURFACE ( 'NONE', #5103, 17.29295143883736330, 7.000000000000003553 ) ;
#2187 = DIRECTION ( 'NONE',  ( -0.01292414190463827932, 0.000000000000000000, -0.9999164797902018176 ) ) ;
#2188 = AXIS2_PLACEMENT_3D ( 'NONE', #17082, #6393, #3045 ) ;
#2189 = CARTESIAN_POINT ( 'NONE',  ( 45.34010913598296355, 168.6466622724117599, 26.02279695137911020 ) ) ;
#2190 = EDGE_CURVE ( 'NONE', #13179, #3953, #100, .T. ) ;
#2191 = EDGE_LOOP ( 'NONE', ( #5795, #8720, #20797, #9896 ) ) ;
#2192 = CARTESIAN_POINT ( 'NONE',  ( 1.054933926688728762, 165.4499317482979279, 81.61824794009152129 ) ) ;
#2193 = ORIENTED_EDGE ( 'NONE', *, *, #8950, .F. ) ;
#2194 = DIRECTION ( 'NONE',  ( -0.01292394549866745720, -0.005513023399720816918, -0.9999012842304692006 ) ) ;
#2195 = CARTESIAN_POINT ( 'NONE',  ( -44.54930311108117280, 173.1906980738792186, 35.16037346336178615 ) ) ;
#2196 = CARTESIAN_POINT ( 'NONE',  ( -74.89818681777818199, 75.00000638978997358, 0.6335213639023836718 ) ) ;
#2197 = CARTESIAN_POINT ( 'NONE',  ( -28.53175067654398234, 324.0509493238391201, 314.6508600760126910 ) ) ;
#2198 = LINE ( 'NONE', #3918, #11033 ) ;
#2199 = EDGE_CURVE ( 'NONE', #18866, #17838, #20635, .T. ) ;
#2200 = CYLINDRICAL_SURFACE ( 'NONE', #3033, 4.374999999999991118 ) ;
#2201 = FACE_OUTER_BOUND ( 'NONE', #15350, .T. ) ;
#2202 = CIRCLE ( 'NONE', #12498, 110.5324305509042233 ) ;
#2203 = CARTESIAN_POINT ( 'NONE',  ( -51.08857079363052378, 110.6671980935713293, -46.33702760430572454 ) ) ;
#2204 = ORIENTED_EDGE ( 'NONE', *, *, #13338, .F. ) ;
#2205 = CYLINDRICAL_SURFACE ( 'NONE', #10574, 2.000000000000001776 ) ;
#2206 = ORIENTED_EDGE ( 'NONE', *, *, #3114, .F. ) ;
#2207 = AXIS2_PLACEMENT_3D ( 'NONE', #18108, #11544, #7746 ) ;
#2208 = ORIENTED_EDGE ( 'NONE', *, *, #19527, .F. ) ;
#2209 = MANIFOLD_SOLID_BREP ( 'Stock-MAS-425-1', #9133 ) ;
#2210 = CARTESIAN_POINT ( 'NONE',  ( -105.1935855565139946, 70.39579207655377502, 32.16088115703475125 ) ) ;
#2211 = TOROIDAL_SURFACE ( 'NONE', #5860, 97.00000000000004263, 2.000000000000000000 ) ;
#2212 = APPLICATION_CONTEXT ( 'automotive_design' ) ;
#2213 = CARTESIAN_POINT ( 'NONE',  ( 17.50001040944635378, 186.7960900973744742, 319.0550816609377875 ) ) ;
#2214 = ADVANCED_FACE ( 'NONE', ( #1361 ), #17099, .T. ) ;
#2215 = PRODUCT_DEFINITION_FORMATION_WITH_SPECIFIED_SOURCE ( 'ANY', '', #19302, .NOT_KNOWN. ) ;
#2216 = EDGE_CURVE ( 'NONE', #16406, #14784, #2886, .T. ) ;
#2217 = ORIENTED_EDGE ( 'NONE', *, *, #964, .T. ) ;
#2218 = AXIS2_PLACEMENT_3D ( 'NONE', #6057, #13192, #15152 ) ;
#2219 = DIRECTION ( 'NONE',  ( -0.9506868100732489557, 0.3101525256269085928, 0.000000000000000000 ) ) ;
#2220 = CARTESIAN_POINT ( 'NONE',  ( -4.209144317661589696, 143.4607783881357932, 276.0169400659812595 ) ) ;
#2221 = DIRECTION ( 'NONE',  ( 7.125109674141484573E-05, -0.9999848031710252272, 0.005512562950851785694 ) ) ;
#2222 = PLANE ( 'NONE',  #9686 ) ;
#2223 = DIRECTION ( 'NONE',  ( 0.000000000000000000, 0.000000000000000000, 1.000000000000000000 ) ) ;
#2224 = CYLINDRICAL_SURFACE ( 'NONE', #10412, 2.000000000000004441 ) ;
#2225 = CARTESIAN_POINT ( 'NONE',  ( 12.89457967643548031, 187.3266554051253081, 305.0022774674998800 ) ) ;
#2226 = CARTESIAN_POINT ( 'NONE',  ( 83.58290648752347352, 104.4142135623730638, 71.51152175067952044 ) ) ;
#2227 = AXIS2_PLACEMENT_3D ( 'NONE', #13603, #8077, #20588 ) ;
#2228 = CARTESIAN_POINT ( 'NONE',  ( -56.11559749965279309, 143.5880916635282176, 107.4801945902891021 ) ) ;
#2229 = EDGE_CURVE ( 'NONE', #10627, #15063, #6736, .T. ) ;
#2230 = ORIENTED_EDGE ( 'NONE', *, *, #2786, .F. ) ;
#2231 = VECTOR ( 'NONE', #10553, 1000.000000000000000 ) ;
#2232 = DIRECTION ( 'NONE',  ( -0.01292394549866754394, -0.005513023399720772683, -0.9999012842304692006 ) ) ;
#2233 = AXIS2_PLACEMENT_3D ( 'NONE', #5351, #5587, #7431 ) ;
#2234 = DIRECTION ( 'NONE',  ( 7.125109674160325297E-05, -0.9999848031710252272, 0.005512562950849327591 ) ) ;
#2235 = ORIENTED_EDGE ( 'NONE', *, *, #9722, .T. ) ;
#2236 = CARTESIAN_POINT ( 'NONE',  ( -93.07689643980960170, 77.12912189501443549, -28.79946631983742833 ) ) ;
#2237 = ORIENTED_EDGE ( 'NONE', *, *, #8286, .F. ) ;
#2238 = FACE_OUTER_BOUND ( 'NONE', #7299, .T. ) ;
#2239 = EDGE_CURVE ( 'NONE', #3243, #7424, #19014, .T. ) ;
#2240 = ADVANCED_BREP_SHAPE_REPRESENTATION ( '', ( #1960, #6292 ), #20203 ) ;
#2241 = AXIS2_PLACEMENT_3D ( 'NONE', #1458, #1567, #9957 ) ;
#2242 = CARTESIAN_POINT ( 'NONE',  ( 51.78636885665599721, 152.2590373701827957, 256.0525387646090394 ) ) ;
#2243 = CARTESIAN_POINT ( 'NONE',  ( 18.63479515211382420, 189.4186551486400845, -105.7525706519799797 ) ) ;
#2244 = VECTOR ( 'NONE', #7831, 1000.000000000000114 ) ;
#2245 = DIRECTION ( 'NONE',  ( 0.01292414190464486780, 0.000000000000000000, 0.9999164797902014845 ) ) ;
#2246 = DIRECTION ( 'NONE',  ( -0.01292394549866738608, -0.005513023399720699824, -0.9999012842304692006 ) ) ;
#2247 = CIRCLE ( 'NONE', #11065, 2.000000000000000000 ) ;
#2248 = DIRECTION ( 'NONE',  ( 0.01292394549866738782, 0.005513023399720700692, 0.9999012842304693116 ) ) ;
#2249 = CARTESIAN_POINT ( 'NONE',  ( 74.41937658727354687, 75.03999983604417423, 1.800753062169240470 ) ) ;
#2250 = FACE_OUTER_BOUND ( 'NONE', #15518, .T. ) ;
#2251 = AXIS2_PLACEMENT_3D ( 'NONE', #18922, #20754, #18816 ) ;
#2252 = ORIENTED_EDGE ( 'NONE', *, *, #17979, .F. ) ;
#2253 = DIRECTION ( 'NONE',  ( -0.9909299940865190504, 0.1338359446631142147, 0.01207007604876868083 ) ) ;
#2254 = ORIENTED_EDGE ( 'NONE', *, *, #19029, .F. ) ;
#2255 = DIRECTION ( 'NONE',  ( -0.4200723624363548736, -0.0005399035332726094451, 0.9074904510909823641 ) ) ;
#2256 = CARTESIAN_POINT ( 'NONE',  ( -48.56578001921132426, 94.99786382055523859, -43.46314047150291060 ) ) ;
#2257 = DIRECTION ( 'NONE',  ( 2.025474946048326158E-22, -1.000000000000000000, 1.876735158486679638E-22 ) ) ;
#2258 = EDGE_CURVE ( 'NONE', #20198, #11876, #3388, .T. ) ;
#2259 = EDGE_CURVE ( 'NONE', #16639, #14542, #2295, .T. ) ;
#2260 = CARTESIAN_POINT ( 'NONE',  ( -90.90343663577488087, 80.03933989046798558, 31.72203358726061495 ) ) ;
#2261 = DIRECTION ( 'NONE',  ( 0.000000000000000000, 1.000000000000000000, -0.000000000000000000 ) ) ;
#2262 = ORIENTED_EDGE ( 'NONE', *, *, #10736, .T. ) ;
#2263 = AXIS2_PLACEMENT_3D ( 'NONE', #17479, #234, #13903 ) ;
#2264 = CARTESIAN_POINT ( 'NONE',  ( 3.808636396294353688, 166.6245905359224082, 294.6670135843256162 ) ) ;
#2265 = AXIS2_PLACEMENT_3D ( 'NONE', #6781, #4820, #15212 ) ;
#2266 = ORIENTED_EDGE ( 'NONE', *, *, #14796, .T. ) ;
#2267 = EDGE_LOOP ( 'NONE', ( #2022, #21934 ) ) ;
#2268 = ORIENTED_EDGE ( 'NONE', *, *, #1239, .T. ) ;
#2269 = CARTESIAN_POINT ( 'NONE',  ( -12.58349991881183172, 105.7167712840407319, 130.3649100882673224 ) ) ;
#2270 = SHAPE_REPRESENTATION ( 'Movable Vise Jaw Block', ( #6292 ), #7747 ) ;
#2271 = CARTESIAN_POINT ( 'NONE',  ( -15.06976562345401227, 178.6172216735134555, 313.9837765850090250 ) ) ;
#2272 = ORIENTED_EDGE ( 'NONE', *, *, #5577, .T. ) ;
#2273 = CONICAL_SURFACE ( 'NONE', #20606, 4.999999999999997335, 0.7853981633974496113 ) ;
#2274 = EDGE_LOOP ( 'NONE', ( #14704, #22602, #20055, #8156, #2494 ) ) ;
#2275 = DIRECTION ( 'NONE',  ( 0.01292394549866738782, 0.005513023399720468239, 0.9999012842304692006 ) ) ;
#2276 = AXIS2_PLACEMENT_3D ( 'NONE', #15101, #6359, #20355 ) ;
#2277 = ORIENTED_EDGE ( 'NONE', *, *, #4000, .F. ) ;
#2278 = CARTESIAN_POINT ( 'NONE',  ( 83.58290648752347352, 104.4142135623730638, 71.51152175067952044 ) ) ;
#2279 = CIRCLE ( 'NONE', #20958, 3.399999999999992806 ) ;
#2280 = AXIS2_PLACEMENT_3D ( 'NONE', #10183, #2943, #9965 ) ;
#2281 = AXIS2_PLACEMENT_3D ( 'NONE', #6633, #2956, #15282 ) ;
#2282 = CARTESIAN_POINT ( 'NONE',  ( -158.3970384574724051, 18.00000000000000355, 62.74304228515463677 ) ) ;
#2283 = DIRECTION ( 'NONE',  ( -0.1136178953597573732, 0.9935164314186356593, -0.004009283626633518283 ) ) ;
#2284 = VERTEX_POINT ( 'NONE', #10846 ) ;
#2285 = CARTESIAN_POINT ( 'NONE',  ( -53.79008187357867854, 126.2575686056374735, 47.53976626672113071 ) ) ;
#2286 = EDGE_CURVE ( 'NONE', #21806, #4488, #16115, .T. ) ;
#2287 = DIRECTION ( 'NONE',  ( -0.01292394549866745720, -0.005513023399720816918, -0.9999012842304692006 ) ) ;
#2288 = ORIENTED_EDGE ( 'NONE', *, *, #7682, .F. ) ;
#2289 = CONICAL_SURFACE ( 'NONE', #22071, 3.399999999999986144, 1.029744258676653201 ) ;
#2290 = EDGE_LOOP ( 'NONE', ( #13159, #19316, #9264 ) ) ;
#2291 = DIRECTION ( 'NONE',  ( -0.01292394549866743465, -0.005513023399721021615, -0.9999012842304692006 ) ) ;
#2292 = LINE ( 'NONE', #12527, #5273 ) ;
#2293 = DIRECTION ( 'NONE',  ( 0.4397038457472340900, 0.000000000000000000, -0.8981428216242072216 ) ) ;
#2294 = LINE ( 'NONE', #580, #18421 ) ;
#2295 = B_SPLINE_CURVE_WITH_KNOTS ( 'NONE', 3,
 ( #21718, #12692, #20000, #21598, #10946, #4039, #21823, #9439, #9566, #9092, #16262, #19660, #16600, #14534, #616, #18199, #14645, #16144, #729, #6004, #5880, #11066, #13137, #4266, #21496, #3927, #18091, #6111, #5760, #11288, #20106, #7725, #2337, #16377, #12918, #19888, #4159, #14763 ),
 .UNSPECIFIED., .F., .F.,
 ( 4, 2, 2, 2, 2, 2, 2, 2, 2, 2, 2, 2, 2, 2, 2, 2, 2, 2, 4 ),
 ( 0.01594779277582532642, 0.01694430233486377002, 0.01794081189390221015, 0.01893732145294065375, 0.01993383101197909388, 0.02093034057101753748, 0.02192685013005597761, 0.02292335968909442120, 0.02391986924813286480, 0.02491637880717130493, 0.02541463358669052500, 0.02591288836620974159, 0.02690939792524816090, 0.02790590748428658369, 0.02890241704332500300, 0.02940067182284419878, 0.02989892660236338762, 0.03089543616140177917, 0.03189194572044016379 ),
 .UNSPECIFIED. ) ;
#2296 = EDGE_LOOP ( 'NONE', ( #15726, #20627 ) ) ;
#2297 = CARTESIAN_POINT ( 'NONE',  ( -101.0000000000000000, 29.00000000000000355, 9.420035382405126825E-16 ) ) ;
#2298 = AXIS2_PLACEMENT_3D ( 'NONE', #3309, #5253, #17221 ) ;
#2299 = AXIS2_PLACEMENT_3D ( 'NONE', #18895, #10594, #12683 ) ;
#2300 = DIRECTION ( 'NONE',  ( 7.125109674364534776E-05, -0.9999848031710252272, 0.005512562950849704893 ) ) ;
#2301 = VERTEX_POINT ( 'NONE', #13701 ) ;
#2302 = DIRECTION ( 'NONE',  ( -0.9999164797902015955, -4.476705744456278510E-15, 0.01292414190463697134 ) ) ;
#2303 = CARTESIAN_POINT ( 'NONE',  ( -88.63691684753834465, 88.68770448415855867, 50.34781501682353877 ) ) ;
#2304 = CONICAL_SURFACE ( 'NONE', #18102, 2.499999999999988010, 1.029744258676651425 ) ;
#2305 = CARTESIAN_POINT ( 'NONE',  ( -121.0618138443797420, 154.6730190510860155, 297.8131875401899720 ) ) ;
#2306 = ORIENTED_EDGE ( 'NONE', *, *, #22096, .F. ) ;
#2307 = CARTESIAN_POINT ( 'NONE',  ( -162.0000000000000000, 18.00000000000000355, 3.967855629237424480E-14 ) ) ;
#2308 = CARTESIAN_POINT ( 'NONE',  ( -38.63447605617402303, 163.9374297322429470, 277.1588331099309812 ) ) ;
#2309 = VERTEX_POINT ( 'NONE', #20349 ) ;
#2310 = FACE_OUTER_BOUND ( 'NONE', #11461, .T. ) ;
#2311 = CARTESIAN_POINT ( 'NONE',  ( 79.99331838321626265, 54.99999999999999289, -1.033931352371318058 ) ) ;
#2312 = ORIENTED_EDGE ( 'NONE', *, *, #2553, .T. ) ;
#2313 = AXIS2_PLACEMENT_3D ( 'NONE', #5602, #8936, #450 ) ;
#2314 = CARTESIAN_POINT ( 'NONE',  ( -105.8297815006158089, 70.09865364193532855, -30.00121230636252889 ) ) ;
#2315 = EDGE_CURVE ( 'NONE', #440, #20401, #15092, .T. ) ;
#2316 = AXIS2_PLACEMENT_3D ( 'NONE', #8607, #13906, #237 ) ;
#2317 = CARTESIAN_POINT ( 'NONE',  ( 51.64670511766545502, 78.91761970611437960, -27.66980033337678790 ) ) ;
#2318 = ORIENTED_EDGE ( 'NONE', *, *, #14884, .T. ) ;
#2319 = CARTESIAN_POINT ( 'NONE',  ( 92.63999567227413934, 77.17622496481537553, 28.88303657775549738 ) ) ;
#2320 = ORIENTED_EDGE ( 'NONE', *, *, #11242, .F. ) ;
#2321 = CARTESIAN_POINT ( 'NONE',  ( 65.34111304903984774, 145.1470193978928478, 25.89384641848939239 ) ) ;
#2322 = CARTESIAN_POINT ( 'NONE',  ( 50.15804862953017818, 189.5999982876588774, -73.26417670677410854 ) ) ;
#2323 = CARTESIAN_POINT ( 'NONE',  ( 157.5176307659771169, 0.000000000000000000, 60.94675664190834397 ) ) ;
#2324 = DIRECTION ( 'NONE',  ( 0.01292394549866738782, 0.005513023399720468239, 0.9999012842304692006 ) ) ;
#2325 = EDGE_CURVE ( 'NONE', #2805, #1815, #22272, .T. ) ;
#2326 = DIRECTION ( 'NONE',  ( 0.9999164797902017066, 6.884683795282953926E-18, -0.01292414190464158570 ) ) ;
#2327 = DIRECTION ( 'NONE',  ( 0.000000000000000000, 0.000000000000000000, -1.000000000000000000 ) ) ;
#2328 = DIRECTION ( 'NONE',  ( 0.9934404589540162256, 0.1135548637187056842, -0.01346653032743081423 ) ) ;
#2329 = CIRCLE ( 'NONE', #4881, 7.500000000000002665 ) ;
#2330 = CARTESIAN_POINT ( 'NONE',  ( 40.15436401027564273, 105.7502092278853496, 91.83706941573649374 ) ) ;
#2331 = ORIENTED_EDGE ( 'NONE', *, *, #17815, .F. ) ;
#2332 = DIRECTION ( 'NONE',  ( 0.000000000000000000, -1.000000000000000000, 0.000000000000000000 ) ) ;
#2333 = CARTESIAN_POINT ( 'NONE',  ( -79.92740525950245001, 75.13699351169597662, 6.133505399301365735 ) ) ;
#2334 = ORIENTED_EDGE ( 'NONE', *, *, #172, .F. ) ;
#2335 = AXIS2_PLACEMENT_3D ( 'NONE', #21523, #7763, #16405 ) ;
#2336 = CIRCLE ( 'NONE', #6376, 6.000000000000003553 ) ;
#2337 = CARTESIAN_POINT ( 'NONE',  ( -82.16334690560557874, 75.11365078037778176, -3.584353236733231807 ) ) ;
#2338 = EDGE_CURVE ( 'NONE', #4798, #2150, #15746, .T. ) ;
#2339 = CARTESIAN_POINT ( 'NONE',  ( -90.16740408589069489, 87.15736368158233915, 51.30261084162481922 ) ) ;
#2340 = VERTEX_POINT ( 'NONE', #16922 ) ;
#2341 = EDGE_CURVE ( 'NONE', #19120, #4209, #20450, .T. ) ;
#2342 = CARTESIAN_POINT ( 'NONE',  ( 39.45263645499988314, 96.15465585523027414, -42.60697859377187058 ) ) ;
#2343 = CIRCLE ( 'NONE', #12636, 8.000000000000000000 ) ;
#2344 = CARTESIAN_POINT ( 'NONE',  ( -92.11907261954638670, 79.08352528315394636, -26.36518256425475570 ) ) ;
#2345 = CARTESIAN_POINT ( 'NONE',  ( -37.41279527276211070, 95.93415318215261323, 85.10526972611022245 ) ) ;
#2346 = DIRECTION ( 'NONE',  ( -0.01292394549866739996, -0.005513023399721131770, -0.9999012842304692006 ) ) ;
#2347 = CARTESIAN_POINT ( 'NONE',  ( 10.82486875048587827, 189.7530090480866534, 275.3475331242451034 ) ) ;
#2348 = CARTESIAN_POINT ( 'NONE',  ( 20.58420809267111196, 182.0421985228920505, 315.9315213838523846 ) ) ;
#2349 = VECTOR ( 'NONE', #2087, 1000.000000000000114 ) ;
#2350 = CARTESIAN_POINT ( 'NONE',  ( 64.42259306105445660, 139.7551263635816952, -45.17031240767400391 ) ) ;
#2351 = ADVANCED_FACE ( 'NONE', ( #22051 ), #8290, .F. ) ;
#2352 = VECTOR ( 'NONE', #6466, 1000.000000000000227 ) ;
#2353 = ADVANCED_FACE ( 'NONE', ( #6353 ), #22381, .F. ) ;
#2354 = DIRECTION ( 'NONE',  ( 0.01035335185279151644, 0.005513005182356664133, 0.9999312050732649393 ) ) ;
#2355 = ORIENTED_EDGE ( 'NONE', *, *, #10784, .T. ) ;
#2356 = EDGE_CURVE ( 'NONE', #6945, #13489, #4994, .T. ) ;
#2357 = EDGE_CURVE ( 'NONE', #10791, #4814, #19010, .T. ) ;
#2358 = DIRECTION ( 'NONE',  ( -0.01292394549866739996, -0.005513023399721131770, -0.9999012842304692006 ) ) ;
#2359 = CARTESIAN_POINT ( 'NONE',  ( -1.163172771417702700, 69.99999999999998579, -89.99248318111824574 ) ) ;
#2360 = ORIENTED_EDGE ( 'NONE', *, *, #21029, .F. ) ;
#2361 = CIRCLE ( 'NONE', #15225, 75.00000000000002842 ) ;
#2362 = DIRECTION ( 'NONE',  ( 0.01292394549866738608, 0.005513023399720699824, 0.9999012842304692006 ) ) ;
#2363 = ORIENTED_EDGE ( 'NONE', *, *, #7383, .T. ) ;
#2364 = ORIENTED_EDGE ( 'NONE', *, *, #7835, .F. ) ;
#2365 = EDGE_CURVE ( 'NONE', #6708, #5718, #20563, .T. ) ;
#2366 = DIRECTION ( 'NONE',  ( 0.01292394549866738782, 0.005513023399720468239, 0.9999012842304692006 ) ) ;
#2367 = AXIS2_PLACEMENT_3D ( 'NONE', #9258, #17674, #1922 ) ;
#2368 = AXIS2_PLACEMENT_3D ( 'NONE', #19561, #16036, #5422 ) ;
#2369 = CARTESIAN_POINT ( 'NONE',  ( -3.467698610696716699, 70.35701968572543308, -99.36756502071496300 ) ) ;
#2370 = EDGE_CURVE ( 'NONE', #19195, #5966, #3250, .T. ) ;
#2371 = CARTESIAN_POINT ( 'NONE',  ( 77.79560129287671089, 75.11063986505354251, 3.580215209361726103 ) ) ;
#2372 = CARTESIAN_POINT ( 'NONE',  ( -90.10530173132328002, 71.17149643761379707, 62.61299491375256565 ) ) ;
#2373 = UNCERTAINTY_MEASURE_WITH_UNIT (LENGTH_MEASURE( 1.000000000000000082E-05 ), #4629, 'distance_accuracy_value', 'NONE');
#2374 = MANIFOLD_SOLID_BREP ( 'Stock-MAS-425-1', #12086 ) ;
#2375 = VERTEX_POINT ( 'NONE', #9900 ) ;
#2376 = DIRECTION ( 'NONE',  ( -0.9999164797902017066, -2.045740421681430110E-15, 0.01292414190464156835 ) ) ;
#2377 = FACE_OUTER_BOUND ( 'NONE', #15801, .T. ) ;
#2378 = FACE_OUTER_BOUND ( 'NONE', #20923, .T. ) ;
#2379 = EDGE_LOOP ( 'NONE', ( #11678, #14418, #11240, #21916 ) ) ;
#2380 = CARTESIAN_POINT ( 'NONE',  ( -39.15186314103204523, 101.1708071963161615, 65.87724253366035043 ) ) ;
#2381 = DIRECTION ( 'NONE',  ( 0.000000000000000000, 0.000000000000000000, 1.000000000000000000 ) ) ;
#2382 = AXIS2_PLACEMENT_3D ( 'NONE', #19722, #16437, #3785 ) ;
#2383 = CARTESIAN_POINT ( 'NONE',  ( 8.332717885210684017, 188.3826505299215057, 276.4169913494580442 ) ) ;
#2384 = EDGE_CURVE ( 'NONE', #11720, #5047, #13476, .T. ) ;
#2385 = CARTESIAN_POINT ( 'NONE',  ( 91.57356387979847057, 79.88289403010834633, -31.31484984389050297 ) ) ;
#2386 = CARTESIAN_POINT ( 'NONE',  ( 0.4472591094132349898, 168.6907664596095628, 34.60359361093173902 ) ) ;
#2387 = CARTESIAN_POINT ( 'NONE',  ( -88.62677304472126139, 79.89796367043616954, 31.25921585370828382 ) ) ;
#2388 = CARTESIAN_POINT ( 'NONE',  ( -10.03308090247307405, 188.0016273849522861, 308.1595840160059083 ) ) ;
#2389 = ORIENTED_EDGE ( 'NONE', *, *, #15150, .F. ) ;
#2390 = CARTESIAN_POINT ( 'NONE',  ( -14.90497309951318883, 180.1700006406394436, 316.7981750502078171 ) ) ;
#2391 = CIRCLE ( 'NONE', #8251, 3.047499999999998987 ) ;
#2392 = ORIENTED_EDGE ( 'NONE', *, *, #22130, .F. ) ;
#2393 = CARTESIAN_POINT ( 'NONE',  ( -53.19758388046658126, 169.4872888238259634, -92.31876405439228961 ) ) ;
#2394 = CARTESIAN_POINT ( 'NONE',  ( -13.80640766535087849, 180.4787919979394530, 308.4662719087184541 ) ) ;
#2395 = ORIENTED_EDGE ( 'NONE', *, *, #11338, .F. ) ;
#2396 = VERTEX_POINT ( 'NONE', #22170 ) ;
#2397 = CARTESIAN_POINT ( 'NONE',  ( -46.77184957787964237, 141.3748088146942621, 250.0790257996952164 ) ) ;
#2398 = CIRCLE ( 'NONE', #8245, 4.200000000000005507 ) ;
#2399 = DIRECTION ( 'NONE',  ( 7.125109674160258889E-05, -0.9999848031710252272, 0.005512562950849896580 ) ) ;
#2400 = EDGE_CURVE ( 'NONE', #1810, #13772, #4705, .T. ) ;
#2401 = CONTEXT_DEPENDENT_SHAPE_REPRESENTATION ( #12366, #10116 ) ;
#2402 = ORIENTED_EDGE ( 'NONE', *, *, #18477, .F. ) ;
#2403 = DIRECTION ( 'NONE',  ( 0.9999164797902015955, 0.000000000000000000, -0.01292414190463754553 ) ) ;
#2404 = LINE ( 'NONE', #9393, #8791 ) ;
#2405 = ORIENTED_EDGE ( 'NONE', *, *, #20018, .F. ) ;
#2406 = CARTESIAN_POINT ( 'NONE',  ( 81.70668847916368804, 104.4142135623730780, -73.64792636435126383 ) ) ;
#2407 = ORIENTED_EDGE ( 'NONE', *, *, #21818, .T. ) ;
#2408 = CARTESIAN_POINT ( 'NONE',  ( 51.12450654134402583, 113.4816418268618037, -44.85357105984766690 ) ) ;
#2409 = ORIENTED_EDGE ( 'NONE', *, *, #5411, .F. ) ;
#2410 = DIRECTION ( 'NONE',  ( 0.01292414190464085018, 1.902755938799529534E-22, 0.9999164797902017066 ) ) ;
#2411 = DIRECTION ( 'NONE',  ( -0.7944560844389302323, 1.242937374672305755E-17, -0.6073216033519337476 ) ) ;
#2412 = VECTOR ( 'NONE', #10464, 1000.000000000000000 ) ;
#2413 = DIRECTION ( 'NONE',  ( 0.1296504907605104673, 0.005475273188900901117, 0.9915446392518421082 ) ) ;
#2414 = DIRECTION ( 'NONE',  ( 0.01292414190464131335, 1.902755938799530239E-22, 0.9999164797902015955 ) ) ;
#2415 = VERTEX_POINT ( 'NONE', #242 ) ;
#2416 = EDGE_LOOP ( 'NONE', ( #17996, #22055, #8671, #13420, #1804, #7996 ) ) ;
#2417 = CARTESIAN_POINT ( 'NONE',  ( 5.448539043597400600, 70.00000000000000000, -83.82247741134344210 ) ) ;
#2418 = CARTESIAN_POINT ( 'NONE',  ( -9.995692194476635706, 187.8898849410517471, 308.1575541326492953 ) ) ;
#2419 = ORIENTED_EDGE ( 'NONE', *, *, #963, .F. ) ;
#2420 = CARTESIAN_POINT ( 'NONE',  ( 41.18571742869637120, 107.5562382960386856, 71.06825843561573208 ) ) ;
#2421 = CARTESIAN_POINT ( 'NONE',  ( -89.66172535072847438, 88.16874122514732903, 50.68101772321399778 ) ) ;
#2422 = EDGE_CURVE ( 'NONE', #12381, #19968, #5049, .T. ) ;
#2423 = DIRECTION ( 'NONE',  ( -0.5075551878391317828, 0.8615475521053163055, -0.01111515896966791539 ) ) ;
#2424 = EDGE_CURVE ( 'NONE', #15988, #5453, #7133, .T. ) ;
#2425 = AXIS2_PLACEMENT_3D ( 'NONE', #20329, #11379, #1040 ) ;
#2426 = ORIENTED_EDGE ( 'NONE', *, *, #4092, .T. ) ;
#2427 = CARTESIAN_POINT ( 'NONE',  ( -4.067676644731616165, 81.92338897118681018, -81.29421751449218903 ) ) ;
#2428 = ORIENTED_EDGE ( 'NONE', *, *, #22655, .T. ) ;
#2429 = CARTESIAN_POINT ( 'NONE',  ( -14.85549656837329557, 175.4877217292663545, 88.65146903140943380 ) ) ;
#2430 = DIRECTION ( 'NONE',  ( 0.01292394549866738782, 0.005513023399720700692, 0.9999012842304693116 ) ) ;
#2431 = CARTESIAN_POINT ( 'NONE',  ( 13.80495188559012121, 157.5998335170374389, 100.8808865402689463 ) ) ;
#2432 = DIRECTION ( 'NONE',  ( 0.01292394549866738608, 0.005513023399720698957, 0.9999012842304692006 ) ) ;
#2433 = ORIENTED_EDGE ( 'NONE', *, *, #20746, .F. ) ;
#2434 = CARTESIAN_POINT ( 'NONE',  ( 91.65137210734579298, 77.59584042966187667, 29.57018005965448637 ) ) ;
#2435 = EDGE_LOOP ( 'NONE', ( #21478, #4282, #13507, #21390 ) ) ;
#2436 = FACE_OUTER_BOUND ( 'NONE', #18984, .T. ) ;
#2437 = CARTESIAN_POINT ( 'NONE',  ( 49.04937187465694137, 189.5912358487612437, -74.83936258294382071 ) ) ;
#2438 = DIRECTION ( 'NONE',  ( -0.9999164797902015955, -2.001050586450176109E-22, 0.01292414190464270113 ) ) ;
#2439 = CARTESIAN_POINT ( 'NONE',  ( 48.56920114533915722, 166.9610289984755127, 276.0150354541233924 ) ) ;
#2440 = DIRECTION ( 'NONE',  ( -2.459148776293844314E-24, 1.000000000000000000, -1.902597020224326827E-22 ) ) ;
#2441 = CARTESIAN_POINT ( 'NONE',  ( -41.07974036897499559, 106.8060942374655156, 71.47017004102838200 ) ) ;
#2442 = CARTESIAN_POINT ( 'NONE',  ( 3.872354045398203937, 166.6517708494369856, 299.5967279023338392 ) ) ;
#2443 = CARTESIAN_POINT ( 'NONE',  ( -44.86761910970069778, 151.3223208568695952, 257.3069776102678929 ) ) ;
#2444 = ORIENTED_EDGE ( 'NONE', *, *, #5205, .T. ) ;
#2445 = B_SPLINE_CURVE_WITH_KNOTS ( 'NONE', 3,
 ( #21074, #14320, #5327, #16050, #7280, #21291 ),
 .UNSPECIFIED., .F., .F.,
 ( 4, 2, 4 ),
 ( 0.000000000000000000, 0.0009922935535326105842, 0.001984587107065221168 ),
 .UNSPECIFIED. ) ;
#2446 = LINE ( 'NONE', #20225, #14996 ) ;
#2447 = ORIENTED_EDGE ( 'NONE', *, *, #1244, .T. ) ;
#2448 = EDGE_CURVE ( 'NONE', #6510, #14770, #19800, .T. ) ;
#2449 = CARTESIAN_POINT ( 'NONE',  ( -90.12718263878197433, 88.36484941033451435, 52.86583380306038293 ) ) ;
#2450 = ADVANCED_FACE ( 'NONE', ( #3340 ), #8714, .F. ) ;
#2451 = EDGE_LOOP ( 'NONE', ( #6970, #1193, #8517, #6199 ) ) ;
#2452 = CARTESIAN_POINT ( 'NONE',  ( 39.88384264372077581, 95.41938954526496275, -43.87626177154204044 ) ) ;
#2453 = CYLINDRICAL_SURFACE ( 'NONE', #20102, 3.099999999999998757 ) ;
#2454 = CARTESIAN_POINT ( 'NONE',  ( -90.39518254297831845, 70.66155102244781006, 61.37085238946110621 ) ) ;
#2455 = PLANE ( 'NONE',  #12630 ) ;
#2456 = DIRECTION ( 'NONE',  ( 0.000000000000000000, 0.000000000000000000, 1.000000000000000000 ) ) ;
#2457 = FACE_OUTER_BOUND ( 'NONE', #21949, .T. ) ;
#2458 = CARTESIAN_POINT ( 'NONE',  ( 20.03694923833142028, 182.5980394464318408, 313.7561223232668794 ) ) ;
#2459 = CARTESIAN_POINT ( 'NONE',  ( 24.46733851482524713, 89.80213272332517249, -79.22137216471709564 ) ) ;
#2460 = EDGE_CURVE ( 'NONE', #12053, #5608, #15014, .T. ) ;
#2461 = CARTESIAN_POINT ( 'NONE',  ( 55.40268456415105902, 1.999999999999998224, -113.1659955246503699 ) ) ;
#2462 = ORIENTED_EDGE ( 'NONE', *, *, #21109, .T. ) ;
#2463 = B_SPLINE_CURVE_WITH_KNOTS ( 'NONE', 3,
 ( #19881, #14417, #19761, #9559, #494, #21491, #4148, #12784, #11059, #18083, #2330, #16372, #9433, #16475, #19032, #15396 ),
 .UNSPECIFIED., .F., .F.,
 ( 4, 2, 2, 2, 2, 2, 2, 4 ),
 ( 0.000000000000000000, 0.0008650928527149638831, 0.001297639279072451083, 0.001730185705429938391, 0.002162732131787425700, 0.002595278558144913008, 0.003027824984502400316, 0.003460371410859887625 ),
 .UNSPECIFIED. ) ;
#2464 =( LENGTH_UNIT ( ) NAMED_UNIT ( * ) SI_UNIT ( .MILLI., .METRE. ) );
#2465 = CARTESIAN_POINT ( 'NONE',  ( -52.96495286149056625, 169.5865232450209703, -74.32054093824388019 ) ) ;
#2466 = DIRECTION ( 'NONE',  ( -0.1296504907605104673, -0.005475273188900901117, -0.9915446392518421082 ) ) ;
#2467 = ORIENTED_EDGE ( 'NONE', *, *, #19157, .F. ) ;
#2468 = CARTESIAN_POINT ( 'NONE',  ( -41.52755568966412625, 166.0426042274538077, 268.7837904884077034 ) ) ;
#2469 = VERTEX_POINT ( 'NONE', #15654 ) ;
#2470 = CARTESIAN_POINT ( 'NONE',  ( 47.42524840967396216, 108.3817487785542824, -44.77763872393808953 ) ) ;
#2471 = VECTOR ( 'NONE', #16768, 1000.000000000000227 ) ;
#2472 = CARTESIAN_POINT ( 'NONE',  ( 40.93051939605364709, 108.3240682923980245, 71.73403676058168799 ) ) ;
#2473 = EDGE_CURVE ( 'NONE', #850, #163, #22598, .T. ) ;
#2474 = ORIENTED_EDGE ( 'NONE', *, *, #8003, .F. ) ;
#2475 = ADVANCED_FACE ( 'NONE', ( #5384 ), #5281, .T. ) ;
#2476 = CARTESIAN_POINT ( 'NONE',  ( 75.53224276191924957, 75.03386225069934312, -3.527861427633645075 ) ) ;
#2477 = CARTESIAN_POINT ( 'NONE',  ( -66.75225376373553843, 145.1029152106950164, 19.60063580020017326 ) ) ;
#2478 = LINE ( 'NONE', #9473, #17026 ) ;
#2479 = LINE ( 'NONE', #16638, #8903 ) ;
#2480 = VERTEX_POINT ( 'NONE', #12323 ) ;
#2481 = DIRECTION ( 'NONE',  ( 7.125109674160258889E-05, -0.9999848031710252272, 0.005512562950849897447 ) ) ;
#2482 = DIRECTION ( 'NONE',  ( 0.000000000000000000, 0.000000000000000000, 1.000000000000000000 ) ) ;
#2483 = FACE_OUTER_BOUND ( 'NONE', #17267, .T. ) ;
#2484 = CARTESIAN_POINT ( 'NONE',  ( -39.85978252003874189, 107.1149823552814269, 71.72844665203564318 ) ) ;
#2485 = AXIS2_PLACEMENT_3D ( 'NONE', #9553, #18186, #13126 ) ;
#2486 = ADVANCED_FACE ( 'NONE', ( #12422 ), #14159, .T. ) ;
#2487 = CARTESIAN_POINT ( 'NONE',  ( 92.43457499998881133, 77.12912189496640281, -31.19724316448931134 ) ) ;
#2488 = DIRECTION ( 'NONE',  ( -0.01292394549866741384, -0.005513023399720270480, -0.9999012842304693116 ) ) ;
#2489 = DIRECTION ( 'NONE',  ( 0.000000000000000000, -0.000000000000000000, 1.000000000000000000 ) ) ;
#2490 = DIRECTION ( 'NONE',  ( 0.9999164797902017066, 0.000000000000000000, -0.01292414190463832269 ) ) ;
#2491 = VERTEX_POINT ( 'NONE', #13914 ) ;
#2492 = CYLINDRICAL_SURFACE ( 'NONE', #61, 3.099999999999998757 ) ;
#2493 = EDGE_CURVE ( 'NONE', #44, #9371, #10596, .T. ) ;
#2494 = ORIENTED_EDGE ( 'NONE', *, *, #1966, .T. ) ;
#2495 = CARTESIAN_POINT ( 'NONE',  ( 22.11217541977124057, 147.9487928221719812, 278.4620210716466886 ) ) ;
#2496 = CARTESIAN_POINT ( 'NONE',  ( -12.36665144395150762, 182.1817021327200621, 309.0434142697981770 ) ) ;
#2497 = ORIENTED_EDGE ( 'NONE', *, *, #10853, .T. ) ;
#2498 = CIRCLE ( 'NONE', #6891, 9.999999999999998224 ) ;
#2499 = EDGE_LOOP ( 'NONE', ( #16336, #18855, #5489, #8445, #12361, #7673 ) ) ;
#2500 = CARTESIAN_POINT ( 'NONE',  ( -40.65822637310711940, 91.17157287525390075, -84.25167897319539634 ) ) ;
#2501 = MECHANICAL_DESIGN_GEOMETRIC_PRESENTATION_REPRESENTATION (  '', ( #4684 ), #16104 ) ;
#2502 = DIRECTION ( 'NONE',  ( 0.01292394549866741557, 0.005513023399720270480, 0.9999012842304693116 ) ) ;
#2503 = EDGE_CURVE ( 'NONE', #1979, #11555, #13540, .T. ) ;
#2504 = B_SPLINE_CURVE_WITH_KNOTS ( 'NONE', 3,
 ( #1357, #18679, #17097, #1255, #18578, #22221, #20631, #1010 ),
 .UNSPECIFIED., .F., .F.,
 ( 4, 2, 2, 4 ),
 ( 0.000000000000000000, 0.002382335671685098782, 0.003573503507527667905, 0.004764671343370237462 ),
 .UNSPECIFIED. ) ;
#2505 = ORIENTED_EDGE ( 'NONE', *, *, #6817, .F. ) ;
#2506 = DIRECTION ( 'NONE',  ( -0.000000000000000000, -1.000000000000000000, 0.000000000000000000 ) ) ;
#2507 = CARTESIAN_POINT ( 'NONE',  ( -53.12424548001075664, 118.8900173874207837, 162.2800983528087215 ) ) ;
#2508 = CIRCLE ( 'NONE', #7273, 83.99999999999998579 ) ;
#2509 = EDGE_LOOP ( 'NONE', ( #11803, #11301, #10423, #14602 ) ) ;
#2510 = FACE_OUTER_BOUND ( 'NONE', #6210, .T. ) ;
#2511 = CARTESIAN_POINT ( 'NONE',  ( -12.68046251919286149, 181.8339994666508233, 307.1133876553329856 ) ) ;
#2512 = VERTEX_POINT ( 'NONE', #3459 ) ;
#2513 = ORIENTED_EDGE ( 'NONE', *, *, #7647, .F. ) ;
#2514 = DIRECTION ( 'NONE',  ( 0.000000000000000000, 1.000000000000000000, 0.000000000000000000 ) ) ;
#2515 = DIRECTION ( 'NONE',  ( -7.125109674025824596E-05, 0.9999848031710253382, -0.005512562950849464634 ) ) ;
#2516 = DIRECTION ( 'NONE',  ( 0.9999164797902015955, 2.001050586498092550E-22, -0.01292414190464117457 ) ) ;
#2517 = CARTESIAN_POINT ( 'NONE',  ( 1.079165849037564184, 69.99999999999998579, 83.49302606248181746 ) ) ;
#2518 = ORIENTED_EDGE ( 'NONE', *, *, #19667, .T. ) ;
#2519 = AXIS2_PLACEMENT_3D ( 'NONE', #5317, #3493, #9099 ) ;
#2520 = EDGE_CURVE ( 'NONE', #11415, #7916, #1737, .T. ) ;
#2521 = DIRECTION ( 'NONE',  ( 0.009760756503427813965, -0.9999378516499565217, 0.005387065077607405654 ) ) ;
#2522 = CARTESIAN_POINT ( 'NONE',  ( -8.523216527044569446, 185.4125284852929099, 305.1540476800932424 ) ) ;
#2523 = ORIENTED_EDGE ( 'NONE', *, *, #6144, .F. ) ;
#2524 = AXIS2_PLACEMENT_3D ( 'NONE', #3123, #22606, #2896 ) ;
#2525 = CARTESIAN_POINT ( 'NONE',  ( 42.65070472731144235, 106.8158425704275771, 70.39662431911894203 ) ) ;
#2526 = EDGE_CURVE ( 'NONE', #18327, #800, #14644, .T. ) ;
#2527 = CARTESIAN_POINT ( 'NONE',  ( -89.41589774379013988, 89.12196685564443044, 51.54718285326051586 ) ) ;
#2528 = ADVANCED_FACE ( 'NONE', ( #5844 ), #5968, .T. ) ;
#2529 = B_SPLINE_CURVE_WITH_KNOTS ( 'NONE', 3,
 ( #15362, #6601, #13629, #1450 ),
 .UNSPECIFIED., .F., .F.,
 ( 4, 4 ),
 ( 2.775557561562891351E-17, 0.0001171670690882713705 ),
 .UNSPECIFIED. ) ;
#2530 = APPLICATION_PROTOCOL_DEFINITION ( 'draft international standard', 'automotive_design', 1998, #21130 ) ;
#2531 = AXIS2_PLACEMENT_3D ( 'NONE', #17874, #3379, #11408 ) ;
#2532 = ORIENTED_EDGE ( 'NONE', *, *, #12333, .F. ) ;
#2533 = CARTESIAN_POINT ( 'NONE',  ( 51.99565694909048830, 170.0000000000000284, -0.6720553790413839046 ) ) ;
#2534 = CARTESIAN_POINT ( 'NONE',  ( -52.09476476361207631, 111.8005892369645551, -46.74040084276866480 ) ) ;
#2535 = ORIENTED_EDGE ( 'NONE', *, *, #3979, .F. ) ;
#2536 = CARTESIAN_POINT ( 'NONE',  ( -48.59517321819919289, 144.7440243326373945, -45.73723683152278596 ) ) ;
#2537 =( BOUNDED_CURVE ( )  B_SPLINE_CURVE ( 3, ( #10708, #5746, #486, #3914 ),
 .UNSPECIFIED., .F., .T. ) 
 B_SPLINE_CURVE_WITH_KNOTS ( ( 4, 4 ),
 ( 1.570796326794896558, 3.141592653589793116 ),
 .UNSPECIFIED. ) 
 CURVE ( )  GEOMETRIC_REPRESENTATION_ITEM ( )  RATIONAL_B_SPLINE_CURVE ( ( 1.000000000000000000, 0.8047378541243649375, 0.8047378541243649375, 1.000000000000000000 ) ) 
 REPRESENTATION_ITEM ( '' )  );
#2538 = DIRECTION ( 'NONE',  ( 0.7070981056135046128, -0.7070960354057282959, -0.005240777737524086356 ) ) ;
#2539 = FACE_OUTER_BOUND ( 'NONE', #362, .T. ) ;
#2540 = CARTESIAN_POINT ( 'NONE',  ( -49.99582398951009310, 170.0000000000008242, 0.6462070952329234119 ) ) ;
#2541 = CARTESIAN_POINT ( 'NONE',  ( 68.71681667565954399, 91.17157287525390075, -85.89527988174788220 ) ) ;
#2542 = ORIENTED_EDGE ( 'NONE', *, *, #17136, .F. ) ;
#2543 = FACE_OUTER_BOUND ( 'NONE', #1026, .T. ) ;
#2544 = ORIENTED_EDGE ( 'NONE', *, *, #19748, .T. ) ;
#2545 = CARTESIAN_POINT ( 'NONE',  ( -49.61360656010212722, 118.9155345184949653, 166.8635573802473857 ) ) ;
#2546 = CARTESIAN_POINT ( 'NONE',  ( 1.741331101896218758, 81.92338897118678176, -98.69074884774437351 ) ) ;
#2547 = DIRECTION ( 'NONE',  ( 0.9232306267972768543, 0.000000000000000000, -0.3842462878721241704 ) ) ;
#2548 = CARTESIAN_POINT ( 'NONE',  ( -38.81723620139342046, 107.2561214313139999, 91.76669763212666453 ) ) ;
#2549 = VECTOR ( 'NONE', #21134, 1000.000000000000000 ) ;
#2550 = EDGE_CURVE ( 'NONE', #17838, #307, #351, .T. ) ;
#2551 = DIRECTION ( 'NONE',  ( 7.125109674403837105E-05, -0.9999848031710252272, 0.005512562950847867821 ) ) ;
#2552 = LINE ( 'NONE', #18082, #11928 ) ;
#2553 = EDGE_CURVE ( 'NONE', #13904, #956, #6408, .T. ) ;
#2554 = CARTESIAN_POINT ( 'NONE',  ( 1.364373935098378649E-14, 105.0000000000000000, -9.836450281572198869E-15 ) ) ;
#2555 = ORIENTED_EDGE ( 'NONE', *, *, #21257, .F. ) ;
#2556 = B_SPLINE_CURVE_WITH_KNOTS ( 'NONE', 3,
 ( #9400, #7573, #5615, #11253, #21665, #14605, #21557, #5832, #4110, #5957, #1265, #1020, #13103, #15390 ),
 .UNSPECIFIED., .F., .F.,
 ( 4, 2, 2, 2, 2, 2, 4 ),
 ( 0.000000000000000000, 0.0009165371227101086048, 0.001374805684065199445, 0.001833074245420290502, 0.002291342806775381342, 0.002749611368130472182, 0.003666148490840745369 ),
 .UNSPECIFIED. ) ;
#2557 = DIRECTION ( 'NONE',  ( 0.01292394549866728373, 0.005513023399720296501, 0.9999012842304693116 ) ) ;
#2558 = ORIENTED_EDGE ( 'NONE', *, *, #5122, .T. ) ;
#2559 = CARTESIAN_POINT ( 'NONE',  ( -105.4170939775132325, 71.46263312473237761, 31.42050039360489677 ) ) ;
#2560 = CARTESIAN_POINT ( 'NONE',  ( -90.16191779797397032, 87.20776688749543837, 51.27200115743783471 ) ) ;
#2561 = CARTESIAN_POINT ( 'NONE',  ( 41.01898768785991933, 92.04141378167193466, 84.43550307159648582 ) ) ;
#2562 = CIRCLE ( 'NONE', #19035, 9.921742784567044282 ) ;
#2563 = ORIENTED_EDGE ( 'NONE', *, *, #14323, .F. ) ;
#2564 = AXIS2_PLACEMENT_3D ( 'NONE', #13742, #1110, #10281 ) ;
#2565 = CARTESIAN_POINT ( 'NONE',  ( -36.94622273008864966, 105.5072037373731888, 92.66402702562507443 ) ) ;
#2566 = CIRCLE ( 'NONE', #4001, 96.00000000000000000 ) ;
#2567 = FACE_OUTER_BOUND ( 'NONE', #10625, .T. ) ;
#2568 = CARTESIAN_POINT ( 'NONE',  ( -2.096375399687102625, 190.2200455327031818, 274.6112675210154634 ) ) ;
#2569 = CARTESIAN_POINT ( 'NONE',  ( 20.36241020427591408, 184.0347753543214537, 278.2158687833079966 ) ) ;
#2570 = CARTESIAN_POINT ( 'NONE',  ( -38.65774199683229284, 93.42233106614874316, 84.97233930033243610 ) ) ;
#2571 = ORIENTED_EDGE ( 'NONE', *, *, #17694, .T. ) ;
#2572 = ORIENTED_EDGE ( 'NONE', *, *, #2056, .F. ) ;
#2573 = FACE_OUTER_BOUND ( 'NONE', #1501, .T. ) ;
#2574 = CARTESIAN_POINT ( 'NONE',  ( 146.4999999999998579, 0.000000000000000000, 10.00000000000199130 ) ) ;
#2575 = CARTESIAN_POINT ( 'NONE',  ( 19.53622439867276128, 183.1519941725404408, 318.8984196516840370 ) ) ;
#2576 = DIRECTION ( 'NONE',  ( 0.9916643202943333790, -7.114886815082621371E-18, 0.1288482667915162028 ) ) ;
#2577 = DIRECTION ( 'NONE',  ( -0.01292394549866740169, -0.005513023399719847208, -0.9999012842304693116 ) ) ;
#2578 = ORIENTED_EDGE ( 'NONE', *, *, #17644, .F. ) ;
#2579 = CARTESIAN_POINT ( 'NONE',  ( 91.26258897903525735, 97.45270810253440175, 61.41003422490156538 ) ) ;
#2580 = VECTOR ( 'NONE', #3755, 1000.000000000000000 ) ;
#2581 = AXIS2_PLACEMENT_3D ( 'NONE', #12804, #21729, #14437 ) ;
#2582 = CARTESIAN_POINT ( 'NONE',  ( 48.56920114533915722, 166.9610289984755127, 276.0150354541233924 ) ) ;
#2583 = CARTESIAN_POINT ( 'NONE',  ( -10.02117361870881851, 187.8727420016839176, 308.1601407300097435 ) ) ;
#2584 = ORIENTED_EDGE ( 'NONE', *, *, #5219, .T. ) ;
#2585 = AXIS2_PLACEMENT_3D ( 'NONE', #10982, #18011, #6047 ) ;
#2586 = CARTESIAN_POINT ( 'NONE',  ( -55.40268456415264353, 1.999999999999998224, -113.1659955246495883 ) ) ;
#2587 = ORIENTED_EDGE ( 'NONE', *, *, #5950, .T. ) ;
#2588 = CARTESIAN_POINT ( 'NONE',  ( 105.4334892372614405, 34.61572286322119396, -31.36525700924962834 ) ) ;
#2589 = VECTOR ( 'NONE', #13773, 999.9999999999998863 ) ;
#2590 = ORIENTED_EDGE ( 'NONE', *, *, #13450, .T. ) ;
#2591 = EDGE_CURVE ( 'NONE', #21410, #20004, #9178, .T. ) ;
#2592 = DIRECTION ( 'NONE',  ( 7.125109674161246868E-05, -0.9999848031710252272, 0.005512562950850154186 ) ) ;
#2593 = LINE ( 'NONE', #7536, #20472 ) ;
#2594 = DIRECTION ( 'NONE',  ( 0.9909299940865187173, -0.1338359446631179062, -0.01207007604876208194 ) ) ;
#2595 = VECTOR ( 'NONE', #19673, 1000.000000000000000 ) ;
#2596 = DIRECTION ( 'NONE',  ( -0.9999164797902017066, -6.965998958219367529E-18, 0.01292414190464157182 ) ) ;
#2597 = AXIS2_PLACEMENT_3D ( 'NONE', #1707, #17111, #10437 ) ;
#2598 = CARTESIAN_POINT ( 'NONE',  ( -3.414999568279890152, 157.2134352445154946, 324.7464257000832504 ) ) ;
#2599 = AXIS2_PLACEMENT_3D ( 'NONE', #22430, #3046, #15141 ) ;
#2600 = ORIENTED_EDGE ( 'NONE', *, *, #22300, .F. ) ;
#2601 = CARTESIAN_POINT ( 'NONE',  ( -36.71973325006338484, -0.3763377030884251795, -67.79345034506853551 ) ) ;
#2602 = CARTESIAN_POINT ( 'NONE',  ( 11.61857788991896179, 160.0893180226940444, 324.5352569096220918 ) ) ;
#2603 = DIRECTION ( 'NONE',  ( -0.01292394549866740690, -0.005513023399721241925, -0.9999012842304693116 ) ) ;
#2604 = EDGE_CURVE ( 'NONE', #21164, #9279, #14390, .T. ) ;
#2605 = CARTESIAN_POINT ( 'NONE',  ( 41.20321018459106455, 119.3672327899910073, 247.5807606757190911 ) ) ;
#2606 = CIRCLE ( 'NONE', #16563, 10.29357798165139393 ) ;
#2607 = DIRECTION ( 'NONE',  ( 2.025474946048326158E-22, -1.000000000000000000, 1.876735158486679638E-22 ) ) ;
#2608 = ORIENTED_EDGE ( 'NONE', *, *, #18607, .F. ) ;
#2609 = EDGE_CURVE ( 'NONE', #922, #8505, #16862, .T. ) ;
#2610 = CARTESIAN_POINT ( 'NONE',  ( 48.56730888123496470, 169.3906321239456361, -111.1677263521955155 ) ) ;
#2611 = ADVANCED_FACE ( 'NONE', ( #19733 ), #11028, .F. ) ;
#2612 = CARTESIAN_POINT ( 'NONE',  ( -110.3452273899772962, 79.04398536104956463, -25.99873445483930823 ) ) ;
#2613 = CARTESIAN_POINT ( 'NONE',  ( -8.886709464532664526, 185.1602439857121283, 307.9998212653392784 ) ) ;
#2614 = EDGE_LOOP ( 'NONE', ( #10124, #11575, #13917, #20807, #7880 ) ) ;
#2615 = ORIENTED_EDGE ( 'NONE', *, *, #14765, .T. ) ;
#2616 = CIRCLE ( 'NONE', #9940, 2.000000000000001776 ) ;
#2617 = CARTESIAN_POINT ( 'NONE',  ( -66.64819547803482180, 98.52889235517193356, 76.44243005894450960 ) ) ;
#2618 = AXIS2_PLACEMENT_3D ( 'NONE', #22365, #10006, #4809 ) ;
#2619 = VECTOR ( 'NONE', #13602, 1000.000000000000114 ) ;
#2620 = CARTESIAN_POINT ( 'NONE',  ( 0.000000000000000000, 0.000000000000000000, 0.000000000000000000 ) ) ;
#2621 = ADVANCED_FACE ( 'NONE', ( #4120 ), #3899, .T. ) ;
#2622 = AXIS2_PLACEMENT_3D ( 'NONE', #9816, #11654, #18649 ) ;
#2623 = EDGE_CURVE ( 'NONE', #1319, #3811, #6197, .T. ) ;
#2624 = CARTESIAN_POINT ( 'NONE',  ( 146.4999999999998579, 0.000000000000000000, -10.00000000000202860 ) ) ;
#2625 = EDGE_CURVE ( 'NONE', #12598, #3397, #14729, .T. ) ;
#2626 = CARTESIAN_POINT ( 'NONE',  ( -2.067862704742604141, 72.00000000000000000, -159.9866367664322979 ) ) ;
#2627 = VERTEX_POINT ( 'NONE', #21239 ) ;
#2628 = DIRECTION ( 'NONE',  ( -0.9232306267972774094, 0.000000000000000000, 0.3842462878721227826 ) ) ;
#2629 = AXIS2_PLACEMENT_3D ( 'NONE', #8985, #37, #17512 ) ;
#2630 = ORIENTED_EDGE ( 'NONE', *, *, #5707, .T. ) ;
#2631 = CARTESIAN_POINT ( 'NONE',  ( -10.22841750353083334, 184.1639157294440565, 305.5386342265414896 ) ) ;
#2632 = ORIENTED_EDGE ( 'NONE', *, *, #20291, .F. ) ;
#2633 = DIRECTION ( 'NONE',  ( 0.000000000000000000, 1.000000000000000000, -0.000000000000000000 ) ) ;
#2634 = CARTESIAN_POINT ( 'NONE',  ( -37.91542670742843057, 96.08856300483259361, 84.97300045992372475 ) ) ;
#2635 = AXIS2_PLACEMENT_3D ( 'NONE', #10926, #21244, #2084 ) ;
#2636 = CARTESIAN_POINT ( 'NONE',  ( -20.87382170032465822, 88.79701099988842827, 78.13772802898489545 ) ) ;
#2637 = ORIENTED_EDGE ( 'NONE', *, *, #20551, .T. ) ;
#2638 = EDGE_CURVE ( 'NONE', #11335, #12812, #9124, .T. ) ;
#2639 = ADVANCED_FACE ( 'NONE', ( #9302 ), #815, .F. ) ;
#2640 = DIRECTION ( 'NONE',  ( -7.125109674118361251E-05, 0.9999848031710253382, -0.005512562950849477644 ) ) ;
#2641 = EDGE_CURVE ( 'NONE', #5358, #1302, #19530, .T. ) ;
#2642 = CARTESIAN_POINT ( 'NONE',  ( -2.000285031460978580, 141.9874903446699363, 256.8043760453134610 ) ) ;
#2643 = VERTEX_POINT ( 'NONE', #11151 ) ;
#2644 = CIRCLE ( 'NONE', #2263, 10.29295143883735619 ) ;
#2645 = DIRECTION ( 'NONE',  ( -1.000000000000000000, 0.000000000000000000, 0.000000000000000000 ) ) ;
#2646 = VECTOR ( 'NONE', #17799, 1000.000000000000114 ) ;
#2647 = CARTESIAN_POINT ( 'NONE',  ( -88.82223701108780745, 89.02496384438940424, 50.89451478405366203 ) ) ;
#2648 = SHAPE_DEFINITION_REPRESENTATION ( #11579, #19567 ) ;
#2649 = EDGE_CURVE ( 'NONE', #12751, #1058, #13221, .T. ) ;
#2650 = EDGE_CURVE ( 'NONE', #9740, #19048, #18597, .T. ) ;
#2651 = ORIENTED_EDGE ( 'NONE', *, *, #16711, .T. ) ;
#2652 = CARTESIAN_POINT ( 'NONE',  ( 0.000000000000000000, 18.00000000000000355, 0.000000000000000000 ) ) ;
#2653 = CARTESIAN_POINT ( 'NONE',  ( -50.37006368079059371, 112.6452800717682408, -43.53711992947328469 ) ) ;
#2654 = EDGE_CURVE ( 'NONE', #18220, #6772, #13448, .T. ) ;
#2655 = CARTESIAN_POINT ( 'NONE',  ( -36.55288090549052527, 94.02752048664899576, 83.45186405039063970 ) ) ;
#2656 = LINE ( 'NONE', #9774, #9230 ) ;
#2657 = AXIS2_PLACEMENT_3D ( 'NONE', #7588, #19862, #10700 ) ;
#2658 = FACE_OUTER_BOUND ( 'NONE', #17459, .T. ) ;
#2659 = CARTESIAN_POINT ( 'NONE',  ( 5.986268468634207807, 81.99999999999998579, -84.52572088931836447 ) ) ;
#2660 = CARTESIAN_POINT ( 'NONE',  ( 88.72067713466825012, 101.8298110126635976, 65.04826529396210333 ) ) ;
#2662 = DIRECTION ( 'NONE',  ( 7.125109674403838460E-05, -0.9999848031710254492, 0.005512562950847868688 ) ) ;
#2661 = APPLICATION_CONTEXT ( 'automotive_design' ) ;
#2663 = EDGE_LOOP ( 'NONE', ( #17888, #15453, #9725, #10215 ) ) ;
#2664 = CARTESIAN_POINT ( 'NONE',  ( 39.40254987707580625, 92.58578643762696458, -84.93055112583746791 ) ) ;
#2665 = VERTEX_POINT ( 'NONE', #7812 ) ;
#2666 = CYLINDRICAL_SURFACE ( 'NONE', #4070, 2.000000000000004885 ) ;
#2667 = FACE_OUTER_BOUND ( 'NONE', #9097, .T. ) ;
#2668 = CARTESIAN_POINT ( 'NONE',  ( -6.065819164189576007, 143.9013245968714045, 275.7904085731360055 ) ) ;
#2669 = CARTESIAN_POINT ( 'NONE',  ( -10.85567112094788200, 105.6999953372425409, 127.2994028633183063 ) ) ;
#2670 = AXIS2_PLACEMENT_3D ( 'NONE', #6925, #14618, #7050 ) ;
#2671 = AXIS2_PLACEMENT_3D ( 'NONE', #6063, #20058, #4320 ) ;
#2672 = ADVANCED_FACE ( 'NONE', ( #1028 ), #13202, .T. ) ;
#2673 = VERTEX_POINT ( 'NONE', #11602 ) ;
#2674 = DIRECTION ( 'NONE',  ( -0.000000000000000000, -1.000000000000000000, -0.000000000000000000 ) ) ;
#2675 = CARTESIAN_POINT ( 'NONE',  ( -10.85340889862633595, 73.95047783656255547, 127.4744267370078177 ) ) ;
#2676 = ORIENTED_EDGE ( 'NONE', *, *, #20858, .F. ) ;
#2677 = CARTESIAN_POINT ( 'NONE',  ( 12.84378735233264379, 190.4863133572641232, 307.8501959441126701 ) ) ;
#2678 = AXIS2_PLACEMENT_3D ( 'NONE', #18936, #20663, #5141 ) ;
#2679 = ORIENTED_EDGE ( 'NONE', *, *, #19298, .F. ) ;
#2680 = ORIENTED_EDGE ( 'NONE', *, *, #16991, .F. ) ;
#2681 = DIRECTION ( 'NONE',  ( -0.009760756503428009989, 0.9999378516499564107, -0.005387065077611111891 ) ) ;
#2682 = CARTESIAN_POINT ( 'NONE',  ( -90.17347746657063112, 87.02151967056039439, 51.38494212375915993 ) ) ;
#2683 =( BOUNDED_CURVE ( )  B_SPLINE_CURVE ( 3, ( #12861, #7800, #5720, #16550 ),
 .UNSPECIFIED., .F., .T. ) 
 B_SPLINE_CURVE_WITH_KNOTS ( ( 4, 4 ),
 ( 4.712388980384689674, 6.283185307179586232 ),
 .UNSPECIFIED. ) 
 CURVE ( )  GEOMETRIC_REPRESENTATION_ITEM ( )  RATIONAL_B_SPLINE_CURVE ( ( 1.000000000000000000, 0.8047378541243649375, 0.8047378541243649375, 1.000000000000000000 ) ) 
 REPRESENTATION_ITEM ( '' )  );
#2684 = AXIS2_PLACEMENT_3D ( 'NONE', #7324, #14136, #21114 ) ;
#2686 = EDGE_LOOP ( 'NONE', ( #15685, #2775, #7795, #11862 ) ) ;
#2685 = ORIENTED_EDGE ( 'NONE', *, *, #19241, .F. ) ;
#2687 = AXIS2_PLACEMENT_3D ( 'NONE', #17748, #8864, #17617 ) ;
#2688 = EDGE_CURVE ( 'NONE', #17908, #4369, #17967, .T. ) ;
#2689 = EDGE_CURVE ( 'NONE', #8292, #21383, #21901, .T. ) ;
#2690 = FACE_OUTER_BOUND ( 'NONE', #20598, .T. ) ;
#2691 = CARTESIAN_POINT ( 'NONE',  ( -91.00106904273528130, 70.29040131071506892, 61.79648398638329354 ) ) ;
#2692 = CARTESIAN_POINT ( 'NONE',  ( -88.63197286364696481, 79.89291707602599502, 31.24418567530317503 ) ) ;
#2693 = DIRECTION ( 'NONE',  ( 7.125109674160258889E-05, -0.9999848031710252272, 0.005512562950849896580 ) ) ;
#2694 = ORIENTED_EDGE ( 'NONE', *, *, #11745, .F. ) ;
#2695 = CARTESIAN_POINT ( 'NONE',  ( 65.44029839719591735, 190.1904397277867531, 33.64500428368677376 ) ) ;
#2696 = FACE_OUTER_BOUND ( 'NONE', #21989, .T. ) ;
#2697 = CARTESIAN_POINT ( 'NONE',  ( 20.06878510934510729, 182.5747025716839289, 314.2333932023548186 ) ) ;
#2698 = DIRECTION ( 'NONE',  ( -7.125109674243555432E-05, 0.9999848031710253382, -0.005512562950850175003 ) ) ;
#2699 = CARTESIAN_POINT ( 'NONE',  ( 54.52327687265658085, 18.00000000000000355, -111.3697098814019171 ) ) ;
#2700 = VECTOR ( 'NONE', #16303, 999.9999999999998863 ) ;
#2701 = VECTOR ( 'NONE', #8952, 999.9999999999998863 ) ;
#2702 = DIRECTION ( 'NONE',  ( 0.01292394549866738782, 0.005513023399720468239, 0.9999012842304692006 ) ) ;
#2703 = LINE ( 'NONE', #13277, #3699 ) ;
#2704 = ORIENTED_EDGE ( 'NONE', *, *, #15287, .F. ) ;
#2705 = CARTESIAN_POINT ( 'NONE',  ( 59.68254426988709582, 143.9326556260109555, 168.4877485356596196 ) ) ;
#2706 = ORIENTED_EDGE ( 'NONE', *, *, #20034, .T. ) ;
#2707 = LINE ( 'NONE', #6142, #1270 ) ;
#2708 = CARTESIAN_POINT ( 'NONE',  ( 41.59766263983357248, 107.1788419875362877, 70.73196411567400332 ) ) ;
#2709 = ORIENTED_EDGE ( 'NONE', *, *, #7404, .F. ) ;
#2710 = AXIS2_PLACEMENT_3D ( 'NONE', #4278, #4171, #18212 ) ;
#2711 = ORIENTED_EDGE ( 'NONE', *, *, #16561, .F. ) ;
#2712 = EDGE_CURVE ( 'NONE', #4144, #14396, #9873, .T. ) ;
#2713 = CARTESIAN_POINT ( 'NONE',  ( 80.05923150692980528, 75.13699351169597662, 4.065642694558706083 ) ) ;
#2714 = DIRECTION ( 'NONE',  ( 0.01292394549866727679, 0.005513023399720742325, 0.9999012842304692006 ) ) ;
#2715 = AXIS2_PLACEMENT_3D ( 'NONE', #10584, #1858, #15899 ) ;
#2716 = VECTOR ( 'NONE', #15104, 1000.000000000000000 ) ;
#2717 = CARTESIAN_POINT ( 'NONE',  ( 75.91984675752824785, 75.11612419797496898, 3.723726926507651580 ) ) ;
#2718 = LINE ( 'NONE', #9477, #19906 ) ;
#2719 = VERTEX_POINT ( 'NONE', #18822 ) ;
#2720 = DIRECTION ( 'NONE',  ( 0.9770372205688161449, -0.2127605332646572978, -0.01145535281434410108 ) ) ;
#2721 = CARTESIAN_POINT ( 'NONE',  ( -0.2071299011688690350, -0.08835629893691807069, -16.02524973528736396 ) ) ;
#2722 = CARTESIAN_POINT ( 'NONE',  ( 1.717753310876221295, 45.00000000000000000, 109.6869605904137330 ) ) ;
#2723 = CARTESIAN_POINT ( 'NONE',  ( 91.47655718793819801, 79.89818662653911474, -31.35069918968699199 ) ) ;
#2724 = FACE_OUTER_BOUND ( 'NONE', #16793, .T. ) ;
#2725 = DIRECTION ( 'NONE',  ( 0.9999164797902017066, 9.297033629063200522E-18, -0.01292414190464145386 ) ) ;
#2726 = VECTOR ( 'NONE', #1050, 1000.000000000000114 ) ;
#2727 = LINE ( 'NONE', #6164, #9216 ) ;
#2728 = PRODUCT_DEFINITION ( 'UNKNOWN', '', #15080, #16177 ) ;
#2729 = ORIENTED_EDGE ( 'NONE', *, *, #9691, .T. ) ;
#2730 = CARTESIAN_POINT ( 'NONE',  ( 12.81503532323078964, 190.4972571607467842, 307.8483445055002221 ) ) ;
#2731 = CARTESIAN_POINT ( 'NONE',  ( -13.29639799380280074, 181.1157429896730946, 307.7937712325852999 ) ) ;
#2732 = ORIENTED_EDGE ( 'NONE', *, *, #17846, .F. ) ;
#2733 = VECTOR ( 'NONE', #17796, 1000.000000000000114 ) ;
#2734 = VERTEX_POINT ( 'NONE', #15182 ) ;
#2735 = CIRCLE ( 'NONE', #6021, 4.999999999999990230 ) ;
#2736 = CARTESIAN_POINT ( 'NONE',  ( -164.0000000000000000, 20.00000000000000000, 0.000000000000000000 ) ) ;
#2737 = AXIS2_PLACEMENT_3D ( 'NONE', #3326, #10348, #10568 ) ;
#2738 = ADVANCED_FACE ( 'NONE', ( #4673 ), #18378, .F. ) ;
#2739 = FACE_OUTER_BOUND ( 'NONE', #22266, .T. ) ;
#2740 = CARTESIAN_POINT ( 'NONE',  ( -10.85567112094788200, 105.6999953372425409, 127.2994028633183063 ) ) ;
#2741 = DIRECTION ( 'NONE',  ( 0.01292394549866760292, 0.005513023399720701559, 0.9999012842304693116 ) ) ;
#2742 = EDGE_LOOP ( 'NONE', ( #5687, #11839, #12737, #13981 ) ) ;
#2743 = AXIS2_PLACEMENT_3D ( 'NONE', #5360, #10324, #14558 ) ;
#2744 = CARTESIAN_POINT ( 'NONE',  ( 3.212670811948540095, 175.3835190792246976, 324.5605796060102648 ) ) ;
#2745 = CARTESIAN_POINT ( 'NONE',  ( -38.79751061739447948, 129.3639651298425406, 248.0419808514072315 ) ) ;
#2746 = VERTEX_POINT ( 'NONE', #16891 ) ;
#2747 = CARTESIAN_POINT ( 'NONE',  ( -59.60610376415444023, 114.2441864440309303, 170.2883384825684061 ) ) ;
#2748 = CARTESIAN_POINT ( 'NONE',  ( -59.21355730958399732, 118.5884715842524173, 107.6580735039648431 ) ) ;
#2749 = PLANE ( 'NONE',  #11819 ) ;
#2750 = EDGE_LOOP ( 'NONE', ( #15186, #17581 ) ) ;
#2751 = EDGE_CURVE ( 'NONE', #11917, #7779, #4721, .T. ) ;
#2752 = EDGE_LOOP ( 'NONE', ( #19574, #8834, #13343, #4593 ) ) ;
#2753 = CARTESIAN_POINT ( 'NONE',  ( -64.33646993259900171, 89.82223348669205620, 51.75612182246453585 ) ) ;
#2754 = DIRECTION ( 'NONE',  ( 2.025474946048326158E-22, -1.000000000000000000, 1.876735158486679638E-22 ) ) ;
#2755 = ADVANCED_FACE ( 'NONE', ( #2757, #16781 ), #8151, .F. ) ;
#2756 = ORIENTED_EDGE ( 'NONE', *, *, #14504, .F. ) ;
#2757 = FACE_BOUND ( 'NONE', #2975, .T. ) ;
#2758 = CARTESIAN_POINT ( 'NONE',  ( 92.40872671617952960, 72.00000000000000000, -33.19707612406970298 ) ) ;
#2759 = APPLICATION_PROTOCOL_DEFINITION ( 'draft international standard', 'automotive_design', 1998, #17182 ) ;
#2760 = EDGE_CURVE ( 'NONE', #307, #17838, #21944, .T. ) ;
#2761 = VERTEX_POINT ( 'NONE', #6436 ) ;
#2762 = DIRECTION ( 'NONE',  ( -0.01035335185279159971, -0.005513005182356926943, -0.9999312050732648283 ) ) ;
#2763 = EDGE_CURVE ( 'NONE', #7115, #14816, #22016, .T. ) ;
#2764 = CARTESIAN_POINT ( 'NONE',  ( -52.45527812472808193, 109.9911275598175280, -43.49553422157452331 ) ) ;
#2765 = CARTESIAN_POINT ( 'NONE',  ( -49.99582398951010731, 170.0000000000000284, 0.6462070952320568828 ) ) ;
#2766 = DIRECTION ( 'NONE',  ( 0.01292394549866727853, 0.005513023399720741458, 0.9999012842304692006 ) ) ;
#2767 = CARTESIAN_POINT ( 'NONE',  ( 146.4999999999998863, 20.00000000000000000, 8.000000000001989520 ) ) ;
#2768 = VERTEX_POINT ( 'NONE', #6082 ) ;
#2769 = DIRECTION ( 'NONE',  ( 0.01292414190464179213, 0.000000000000000000, 0.9999164797902017066 ) ) ;
#2770 = PRODUCT_DEFINITION_SHAPE ( 'NONE', 'NONE',  #9157 ) ;
#2771 = CARTESIAN_POINT ( 'NONE',  ( 51.64670511766545502, 84.99999999999997158, -27.66980033337678790 ) ) ;
#2772 = LINE ( 'NONE', #8163, #4173 ) ;
#2773 = VERTEX_POINT ( 'NONE', #16681 ) ;
#2774 = CARTESIAN_POINT ( 'NONE',  ( 34.67902741341890760, 93.81357993601811529, -83.23127688097689258 ) ) ;
#2775 = ORIENTED_EDGE ( 'NONE', *, *, #22047, .F. ) ;
#2776 = PLANE ( 'NONE',  #1877 ) ;
#2777 = CARTESIAN_POINT ( 'NONE',  ( 86.79222083800954124, 104.3814432989690602, 67.58039954014910222 ) ) ;
#2778 = CARTESIAN_POINT ( 'NONE',  ( -38.92003986412552052, 97.39926864640099780, 83.81297216957182172 ) ) ;
#2779 = CARTESIAN_POINT ( 'NONE',  ( -9.472248412593200939, 69.99999999999998579, -86.53426659026914081 ) ) ;
#2780 = EDGE_CURVE ( 'NONE', #13067, #2773, #20502, .T. ) ;
#2781 = ORIENTED_EDGE ( 'NONE', *, *, #2751, .F. ) ;
#2782 = CARTESIAN_POINT ( 'NONE',  ( 84.03923162725097029, 104.9999999999999858, -70.97549463945256321 ) ) ;
#2783 = CARTESIAN_POINT ( 'NONE',  ( -57.55251350461809778, 118.9484885890504557, 172.9440730829682877 ) ) ;
#2784 = ORIENTED_EDGE ( 'NONE', *, *, #18556, .F. ) ;
#2785 = CARTESIAN_POINT ( 'NONE',  ( 13.84903886101111681, 155.5756827379013885, 104.2918126654085995 ) ) ;
#2786 = EDGE_CURVE ( 'NONE', #22376, #17867, #11350, .T. ) ;
#2787 = DIRECTION ( 'NONE',  ( 0.9999164797902017066, 6.965998958219365988E-18, -0.01292414190464157356 ) ) ;
#2788 = ORIENTED_EDGE ( 'NONE', *, *, #16045, .T. ) ;
#2789 = AXIS2_PLACEMENT_3D ( 'NONE', #17496, #20802, #6796 ) ;
#2790 = FILL_AREA_STYLE_COLOUR ( '', #9106 ) ;
#2791 = CARTESIAN_POINT ( 'NONE',  ( -90.12564631705923546, 88.34868647126225483, 52.87392178893500727 ) ) ;
#2792 = DIRECTION ( 'NONE',  ( -0.9999164797902017066, -2.457127383503899093E-15, 0.01292414190464056742 ) ) ;
#2793 = VERTEX_POINT ( 'NONE', #18700 ) ;
#2794 = EDGE_CURVE ( 'NONE', #22165, #19122, #2972, .T. ) ;
#2795 = CARTESIAN_POINT ( 'NONE',  ( 59.65023440614042727, 143.9188730675116688, 165.9879953250834603 ) ) ;
#2796 = DIRECTION ( 'NONE',  ( 0.01292394549866738782, 0.005513023399720468239, 0.9999012842304692006 ) ) ;
#2797 = DIRECTION ( 'NONE',  ( 7.125109674364534776E-05, -0.9999848031710252272, 0.005512562950849704893 ) ) ;
#2798 = FACE_OUTER_BOUND ( 'NONE', #20156, .T. ) ;
#2799 = LINE ( 'NONE', #6575, #13371 ) ;
#2800 = ORIENTED_EDGE ( 'NONE', *, *, #15005, .F. ) ;
#2801 = DIRECTION ( 'NONE',  ( 0.01292414190464044946, 1.902755938799528593E-22, 0.9999164797902015955 ) ) ;
#2802 = CARTESIAN_POINT ( 'NONE',  ( 20.39811478720299220, 182.2549943958479446, 316.7388195023896742 ) ) ;
#2803 = LINE ( 'NONE', #7743, #16222 ) ;
#2804 = DIRECTION ( 'NONE',  ( 7.125109674160325297E-05, -0.9999848031710253382, 0.005512562950849327591 ) ) ;
#2805 = VERTEX_POINT ( 'NONE', #4793 ) ;
#2806 = CARTESIAN_POINT ( 'NONE',  ( 0.000000000000000000, 0.000000000000000000, 0.000000000000000000 ) ) ;
#2807 = EDGE_CURVE ( 'NONE', #13285, #8542, #5246, .T. ) ;
#2808 = DIRECTION ( 'NONE',  ( 0.9910138020846641638, -0.1337596504095987238, 0.000000000000000000 ) ) ;
#2809 =( BOUNDED_SURFACE ( )  B_SPLINE_SURFACE ( 3, 2, ( 
 ( #6226, #16378, #11402 ),
 ( #9568, #6005, #2682 ),
 ( #1065, #4267, #18414 ),
 ( #11067, #18092, #962 ),
 ( #6113, #11290, #4495 ),
 ( #13138, #7948, #21824 ),
 ( #13255, #5882, #11526 ),
 ( #14979, #13044, #9690 ),
 ( #19889, #20107, #20231 ),
 ( #4374, #7727, #8055 ),
 ( #16714, #4160, #21599 ),
 ( #18529, #5761, #21931 ),
 ( #12792, #21497, #2339 ),
 ( #12919, #2791, #11184 ),
 ( #18200, #2449, #9440 ),
 ( #618, #16481, #20002 ),
 ( #18298, #7609, #2560 ),
 ( #9796, #16601, #852 ),
 ( #16812, #14880, #17371 ),
 ( #15095, #6354, #20565 ),
 ( #3342, #18738, #15323 ),
 ( #22273, #8500, #13703 ),
 ( #20350, #10022, #4940 ),
 ( #1631, #22495, #18957 ),
 ( #5050, #13477, #20451 ),
 ( #4608, #17251, #20794 ),
 ( #4825, #12081, #11740 ),
 ( #1520, #15433, #11863 ),
 ( #22171, #19069, #10362 ),
 ( #8291, #3216, #17142 ),
 ( #22383, #6784, #11633 ),
 ( #18626, #4706, #6566 ),
 ( #22052, #6465, #13582 ),
 ( #18854, #13374, #6676 ),
 ( #10241, #1308, #3117 ),
 ( #16924, #2888, #9902 ),
 ( #1190, #8186, #1410 ),
 ( #15217, #10135, #3001 ),
 ( #17045, #8389, #20687 ),
 ( #11976, #15543, #13809 ),
 ( #5282, #10920, #17941 ),
 ( #9059, #21139, #8960 ),
 ( #1847, #12662, #19301 ),
 ( #2079, #7237, #19531 ),
 ( #16006, #8614, #3797 ),
 ( #10576, #17600, #8843 ),
 ( #15889, #14043, #12424 ),
 ( #8716, #5385, #16112 ),
 ( #10473, #354, #19188 ),
 ( #10693, #10, #7015 ),
 ( #14266, #21028, #3672 ),
 ( #19633, #3565, #14392 ),
 ( #3460, #12536, #12324 ),
 ( #15655, #17722, #3900 ),
 ( #133, #7345, #21241 ),
 ( #13915, #243, #22600 ),
 ( #1970, #7134, #14160 ),
 ( #20907, #19410, #5506 ),
 ( #10822, #15769, #17841 ),
 ( #6893, #17487, #21356 ),
 ( #5628, #5164, #12204 ),
 ( #1738, #16449, #5845 ),
 ( #7470, #13222, #19852 ),
 ( #18379, #9531, #11152 ),
 ( #13109, #14953, #9656 ),
 ( #14845, #2527, #13006 ),
 ( #6083, #4004, #21902 ),
 ( #588, #18270, #4343 ),
 ( #4465, #16566, #12875 ),
 ( #6194, #20079, #19971 ),
 ( #18170, #817, #4237 ),
 ( #20195, #11370, #2421 ),
 ( #11261, #7581, #7813 ),
 ( #21468, #21793, #9410 ),
 ( #21567, #2647, #14613 ),
 ( #18056, #5969, #16682 ),
 ( #931, #4121, #9179 ),
 ( #16232, #471, #2303 ),
 ( #9303, #697, #7691 ),
 ( #14730, #19734, #12762 ) ),
 .UNSPECIFIED., .F., .F., .T. ) 
 B_SPLINE_SURFACE_WITH_KNOTS ( ( 4, 2, 2, 2, 2, 2, 2, 2, 2, 2, 2, 2, 2, 2, 2, 2, 2, 2, 2, 2, 2, 2, 2, 2, 2, 2, 2, 2, 2, 2, 2, 2, 2, 2, 2, 2, 2, 2, 2, 4 ),
 ( 3, 3 ),
 ( 1.949022811632145080E-18, 1.486245462785398132E-07, 2.972490925551306036E-07, 4.458736388317213675E-07, 5.944981851083121843E-07, 7.431227313849028953E-07, 8.917472776614937121E-07, 1.040371823938084529E-06, 1.188996370214675346E-06, 1.337620916491266163E-06, 1.486245462767856768E-06, 1.634870009044447585E-06, 1.783494555321038401E-06, 1.932119101597629430E-06, 2.080743647874220035E-06, 2.229368194150810640E-06, 2.377992740427401669E-06, 2.526617286703992697E-06, 2.675241832980583302E-06, 2.823866379257173908E-06, 2.898178652395469210E-06, 2.972490925533764513E-06, 3.269740018086946146E-06, 3.566989110640127780E-06, 3.864238203193308990E-06, 4.161487295746491047E-06, 4.458736388299673105E-06, 4.755985480852854315E-06, 5.053234573406035525E-06, 5.350483665959217582E-06, 5.647732758512399639E-06, 5.944981851065580850E-06, 6.242230943618762060E-06, 6.539480036171944117E-06, 6.836729128725126174E-06, 7.133978221278307384E-06, 9.511970961703760454E-06, 1.188996370212921352E-05, 1.426795644255466659E-05, 1.902394192340557273E-05 ),
 ( 0.000000000000000000, 1.000000000000000000 ),
 .UNSPECIFIED. ) 
 GEOMETRIC_REPRESENTATION_ITEM ( )  RATIONAL_B_SPLINE_SURFACE ( (
 ( 1.000000000000000000, 0.7071067811865135999, 1.000000000000000000),
 ( 1.000000000000000000, 0.7072381281680633069, 1.000000000000000000),
 ( 1.000000000000000000, 0.7069585476545049429, 1.000000000000000000),
 ( 1.000000000000000000, 0.7074155413819450677, 1.000000000000000000),
 ( 1.000000000000000000, 0.7071390384860228862, 1.000000000000000000),
 ( 1.000000000000000000, 0.7077150574724885290, 1.000000000000000000),
 ( 1.000000000000000000, 0.7074786063547826576, 1.000000000000000000),
 ( 1.000000000000000000, 0.7081708585959944902, 1.000000000000000000),
 ( 1.000000000000000000, 0.7079751951990761460, 1.000000000000000000),
 ( 1.000000000000000000, 0.7087807454553832764, 1.000000000000000000),
 ( 1.000000000000000000, 0.7086266733915456140, 1.000000000000000000),
 ( 1.000000000000000000, 0.7095424613801466496, 1.000000000000000000),
 ( 1.000000000000000000, 0.7094308370090658400, 1.000000000000000000),
 ( 1.000000000000000000, 0.7104536936552536819, 1.000000000000000000),
 ( 1.000000000000000000, 0.7103854132845832670, 1.000000000000000000),
 ( 1.000000000000000000, 0.7115120753684263111, 1.000000000000000000),
 ( 1.000000000000000000, 0.7114880643480506750, 1.000000000000000000),
 ( 1.000000000000000000, 0.7127151874304157309, 1.000000000000000000),
 ( 1.000000000000000000, 0.7127363908997321751, 1.000000000000000000),
 ( 1.000000000000000000, 0.7140605608518137970, 1.000000000000000000),
 ( 1.000000000000000000, 0.7141279362315575696, 1.000000000000000000),
 ( 1.000000000000000000, 0.7155456793979033669, 1.000000000000000000),
 ( 1.000000000000000000, 0.7156601900754941958, 1.000000000000000000),
 ( 1.000000000000000000, 0.7171679822068535159, 1.000000000000000000),
 ( 1.000000000000000000, 0.7173305926685255018, 1.000000000000000000),
 ( 1.000000000000000000, 0.7189248667156663553, 1.000000000000000000),
 ( 1.000000000000000000, 0.7191365387466063241, 1.000000000000000000),
 ( 1.000000000000000000, 0.7208136916140887029, 1.000000000000000000),
 ( 1.000000000000000000, 0.7210753815884107798, 1.000000000000000000),
 ( 1.000000000000000000, 0.7228317799310683966, 1.000000000000000000),
 ( 1.000000000000000000, 0.7231444369243380521, 1.000000000000000000),
 ( 1.000000000000000000, 0.7249764221348216076, 1.000000000000000000),
 ( 1.000000000000000000, 0.7253410135264871661, 1.000000000000000000),
 ( 1.000000000000000000, 0.7272448526125560031, 1.000000000000000000),
 ( 1.000000000000000000, 0.7276627513310924833, 1.000000000000000000),
 ( 1.000000000000000000, 0.7296339184630242780, 1.000000000000000000),
 ( 1.000000000000000000, 0.7301067830575730389, 1.000000000000000000),
 ( 1.000000000000000000, 0.7321408070295029047, 1.000000000000000000),
 ( 1.000000000000000000, 0.7326585513427095187, 1.000000000000000000),
 ( 1.000000000000000000, 0.7342303961178014982, 1.000000000000000000),
 ( 1.000000000000000000, 0.7345026836460134545, 1.000000000000000000),
 ( 1.000000000000000000, 0.7355652195318463926, 1.000000000000000000),
 ( 1.000000000000000000, 0.7359821834485184011, 1.000000000000000000),
 ( 1.000000000000000000, 0.7379952682253708707, 1.000000000000000000),
 ( 1.000000000000000000, 0.7402826106793318761, 1.000000000000000000),
 ( 1.000000000000000000, 0.7437381524183488413, 1.000000000000000000),
 ( 1.000000000000000000, 0.7461303745155040135, 1.000000000000000000),
 ( 1.000000000000000000, 0.7498005034201070673, 1.000000000000000000),
 ( 1.000000000000000000, 0.7522845452621365059, 1.000000000000000000),
 ( 1.000000000000000000, 0.7561493072734657428, 1.000000000000000000),
 ( 1.000000000000000000, 0.7587139551311251617, 1.000000000000000000),
 ( 1.000000000000000000, 0.7627534639691019303, 1.000000000000000000),
 ( 1.000000000000000000, 0.7653892180658008471, 1.000000000000000000),
 ( 1.000000000000000000, 0.7695836597282257330, 1.000000000000000000),
 ( 1.000000000000000000, 0.7722826061538781151, 1.000000000000000000),
 ( 1.000000000000000000, 0.7766122452106001273, 1.000000000000000000),
 ( 1.000000000000000000, 0.7793679326086000447, 1.000000000000000000),
 ( 1.000000000000000000, 0.7838131199424147599, 1.000000000000000000),
 ( 1.000000000000000000, 0.7866200293621847806, 1.000000000000000000),
 ( 1.000000000000000000, 0.7911602176995968794, 1.000000000000000000),
 ( 1.000000000000000000, 0.7939709014748255189, 1.000000000000000000),
 ( 1.000000000000000000, 0.7985820451014939980, 1.000000000000000000),
 ( 1.000000000000000000, 0.8013687969964130575, 1.000000000000000000),
 ( 1.000000000000000000, 0.8060341433133167977, 1.000000000000000000),
 ( 1.000000000000000000, 0.8087928835127498051, 1.000000000000000000),
 ( 1.000000000000000000, 0.8134970145047152323, 1.000000000000000000),
 ( 1.000000000000000000, 0.8162250625491064282, 1.000000000000000000),
 ( 1.000000000000000000, 0.8209521604033785946, 1.000000000000000000),
 ( 1.000000000000000000, 0.8236482853497503198, 1.000000000000000000),
 ( 1.000000000000000000, 0.8283833078820742601, 1.000000000000000000),
 ( 1.000000000000000000, 0.8309614497935257083, 1.000000000000000000),
 ( 1.000000000000000000, 0.8530099714809558087, 1.000000000000000000),
 ( 1.000000000000000000, 0.8723999263078645594, 1.000000000000000000),
 ( 1.000000000000000000, 0.9074054958599828691, 1.000000000000000000),
 ( 1.000000000000000000, 0.9231958273998440712, 1.000000000000000000),
 ( 1.000000000000000000, 0.9505426722021091956, 1.000000000000000000),
 ( 1.000000000000000000, 0.9622396665221361056, 1.000000000000000000),
 ( 1.000000000000000000, 0.9904446952675073357, 1.000000000000000000),
 ( 1.000000000000000000, 1.000033919101930513, 1.000000000000000000),
 ( 1.000000000000000000, 1.000000000000000000, 1.000000000000000000) ) ) 
 REPRESENTATION_ITEM ( '' )  SURFACE ( )  );
#2810 = CARTESIAN_POINT ( 'NONE',  ( 49.99582398951009310, 170.0000000000008242, -0.6462070952312342076 ) ) ;
#2811 = VERTEX_POINT ( 'NONE', #1380 ) ;
#2812 = DIRECTION ( 'NONE',  ( 0.000000000000000000, 0.000000000000000000, -1.000000000000000000 ) ) ;
#2813 = EDGE_LOOP ( 'NONE', ( #15309, #12745 ) ) ;
#2814 = FACE_OUTER_BOUND ( 'NONE', #11527, .T. ) ;
#2815 = ORIENTED_EDGE ( 'NONE', *, *, #2356, .T. ) ;
#2816 = ADVANCED_FACE ( 'NONE', ( #10210 ), #6577, .F. ) ;
#2817 = PRESENTATION_STYLE_ASSIGNMENT (( #8315 ) ) ;
#2818 = CARTESIAN_POINT ( 'NONE',  ( -34.98828874231188735, 165.2145695649813888, 276.3045847542423417 ) ) ;
#2819 = CARTESIAN_POINT ( 'NONE',  ( 105.5195728421876140, 78.18109283220586292, -31.07451122637847973 ) ) ;
#2820 = FACE_OUTER_BOUND ( 'NONE', #11515, .T. ) ;
#2821 = CARTESIAN_POINT ( 'NONE',  ( 19.19569574945376544, 186.7745716580498367, 276.1480060676194057 ) ) ;
#2822 = ORIENTED_EDGE ( 'NONE', *, *, #16123, .F. ) ;
#2823 =( NAMED_UNIT ( * ) SI_UNIT ( $, .STERADIAN. ) SOLID_ANGLE_UNIT ( ) );
#2824 = CARTESIAN_POINT ( 'NONE',  ( 41.99649215118846968, 170.0000000000000284, -0.5428139599949681759 ) ) ;
#2825 = DIRECTION ( 'NONE',  ( 0.009760756503428009989, -0.9999378516499564107, 0.005387065077611111891 ) ) ;
#2826 = CARTESIAN_POINT ( 'NONE',  ( -41.00865927789263310, 166.2639521169525665, 308.9298270502609967 ) ) ;
#2827 = CARTESIAN_POINT ( 'NONE',  ( 91.90296438722727146, 77.16966923688237046, -31.25747399733695175 ) ) ;
#2828 = CARTESIAN_POINT ( 'NONE',  ( 92.21925947168416826, 70.54513337289785113, 59.96440893983636755 ) ) ;
#2829 = FACE_OUTER_BOUND ( 'NONE', #2614, .T. ) ;
#2830 = ORIENTED_EDGE ( 'NONE', *, *, #1925, .T. ) ;
#2831 = ORIENTED_EDGE ( 'NONE', *, *, #1101, .T. ) ;
#2832 = EDGE_CURVE ( 'NONE', #5236, #822, #17460, .T. ) ;
#2833 = CARTESIAN_POINT ( 'NONE',  ( -38.27775742616200461, 165.9786531560170033, 257.1409935088582870 ) ) ;
#2834 = CARTESIAN_POINT ( 'NONE',  ( -12.67437722926222143, 184.6792686180227179, 309.1546888890629816 ) ) ;
#2835 = ADVANCED_FACE ( 'NONE', ( #11945 ), #19036, .T. ) ;
#2836 = VERTEX_POINT ( 'NONE', #10327 ) ;
#2837 = VERTEX_POINT ( 'NONE', #14005 ) ;
#2838 = CARTESIAN_POINT ( 'NONE',  ( -67.52146002153369864, 70.28876377827108968, 86.83823687282564663 ) ) ;
#2839 = EDGE_LOOP ( 'NONE', ( #21238, #1221, #2402, #11138 ) ) ;
#2840 = CARTESIAN_POINT ( 'NONE',  ( 79.99331838321626265, 102.0000000000000000, 4.966068647628683053 ) ) ;
#2841 = VECTOR ( 'NONE', #2438, 1000.000000000000114 ) ;
#2842 = CARTESIAN_POINT ( 'NONE',  ( 20.70083805927511733, 149.3646325075532957, 278.4026507072620120 ) ) ;
#2843 = PLANE ( 'NONE',  #19899 ) ;
#2844 = VERTEX_POINT ( 'NONE', #19272 ) ;
#2845 = DIRECTION ( 'NONE',  ( 0.1136178953597579561, -0.9935164314186356593, 0.004009283626633661397 ) ) ;
#2846 = FACE_OUTER_BOUND ( 'NONE', #10676, .T. ) ;
#2847 = CARTESIAN_POINT ( 'NONE',  ( -106.2089377515398780, 34.61572286322119396, -28.62973177816246206 ) ) ;
#2848 = CARTESIAN_POINT ( 'NONE',  ( 7.825680009415360239, 70.07756262466202202, -91.81739557479740199 ) ) ;
#2849 = CARTESIAN_POINT ( 'NONE',  ( -2.096375399687102625, 190.2200455327031818, 274.6112675210154634 ) ) ;
#2850 = ORIENTED_EDGE ( 'NONE', *, *, #15533, .F. ) ;
#2851 = DIRECTION ( 'NONE',  ( 7.125109674364534776E-05, -0.9999848031710252272, 0.005512562950849704893 ) ) ;
#2852 = EDGE_CURVE ( 'NONE', #1571, #21136, #15624, .T. ) ;
#2853 = FACE_BOUND ( 'NONE', #15218, .T. ) ;
#2854 = CARTESIAN_POINT ( 'NONE',  ( 14.71507153966036974, 144.4759177913303745, 275.7214514730162591 ) ) ;
#2855 = AXIS2_PLACEMENT_3D ( 'NONE', #20215, #4481, #11512 ) ;
#2856 = CARTESIAN_POINT ( 'NONE',  ( 0.000000000000000000, 37.00000000000000711, 0.000000000000000000 ) ) ;
#2857 = VERTEX_POINT ( 'NONE', #3537 ) ;
#2858 = DIRECTION ( 'NONE',  ( -0.01292394549866741384, -0.005513023399720269613, -0.9999012842304692006 ) ) ;
#2859 = DIRECTION ( 'NONE',  ( -1.000000000000000000, -0.000000000000000000, -0.000000000000000000 ) ) ;
#2860 = CONTEXT_DEPENDENT_SHAPE_REPRESENTATION ( #9711, #21121 ) ;
#2861 = VECTOR ( 'NONE', #13577, 1000.000000000000114 ) ;
#2862 = ORIENTED_EDGE ( 'NONE', *, *, #19183, .F. ) ;
#2863 = EDGE_CURVE ( 'NONE', #3975, #21200, #16504, .T. ) ;
#2864 = CARTESIAN_POINT ( 'NONE',  ( -51.07137216368364818, 109.3042685136236685, -43.50963446871423201 ) ) ;
#2865 = ORIENTED_EDGE ( 'NONE', *, *, #17744, .F. ) ;
#2866 = DIRECTION ( 'NONE',  ( 5.257943380984030796E-16, -1.000000000000000000, -6.795817950787834712E-18 ) ) ;
#2867 = CARTESIAN_POINT ( 'NONE',  ( -1.421655609510530827, 69.99999999999998579, -109.9908127769221693 ) ) ;
#2868 = FACE_OUTER_BOUND ( 'NONE', #7162, .T. ) ;
#2869 = LINE ( 'NONE', #11958, #17891 ) ;
#2870 = AXIS2_PLACEMENT_3D ( 'NONE', #19684, #17787, #2025 ) ;
#2871 = CARTESIAN_POINT ( 'NONE',  ( 44.03028354117878251, 168.0879242961143518, -75.31593853751020617 ) ) ;
#2872 = EDGE_LOOP ( 'NONE', ( #21707, #2149, #8412 ) ) ;
#2873 = LINE ( 'NONE', #11721, #21268 ) ;
#2874 = ORIENTED_EDGE ( 'NONE', *, *, #6944, .F. ) ;
#2875 = DIRECTION ( 'NONE',  ( -0.9934404589540162256, -0.1135548637187059617, 0.01346653032742970747 ) ) ;
#2876 = CARTESIAN_POINT ( 'NONE',  ( 86.63143169152132828, 104.5954341936825642, 67.78689798060398175 ) ) ;
#2877 = CARTESIAN_POINT ( 'NONE',  ( 105.7217631510340965, 70.01235472379877933, 30.37969943364865699 ) ) ;
#2878 = DIRECTION ( 'NONE',  ( 0.4910069343201003411, -0.004767316193522950878, -0.8711426192914037969 ) ) ;
#2879 = LINE ( 'NONE', #6666, #10748 ) ;
#2880 = CARTESIAN_POINT ( 'NONE',  ( 18.04061865414768207, 188.1738179166474367, 322.2972073689282979 ) ) ;
#2881 = ADVANCED_FACE ( 'NONE', ( #20762 ), #17342, .T. ) ;
#2882 = ORIENTED_EDGE ( 'NONE', *, *, #18755, .F. ) ;
#2883 = DIRECTION ( 'NONE',  ( -0.01292394549866740169, -0.005513023399721131770, -0.9999012842304693116 ) ) ;
#2884 = EDGE_CURVE ( 'NONE', #17869, #6385, #19760, .T. ) ;
#2885 = DIRECTION ( 'NONE',  ( -0.000000000000000000, 1.000000000000000000, -0.000000000000000000 ) ) ;
#2886 = CIRCLE ( 'NONE', #5446, 7.500000000000002665 ) ;
#2887 = ORIENTED_EDGE ( 'NONE', *, *, #2763, .F. ) ;
#2888 = CARTESIAN_POINT ( 'NONE',  ( -89.97698801024371562, 88.76047946969235625, 52.44252181446705663 ) ) ;
#2889 = CARTESIAN_POINT ( 'NONE',  ( 41.58451242677342918, 92.58578643762696458, 83.88377541325536413 ) ) ;
#2891 = ORIENTED_EDGE ( 'NONE', *, *, #10175, .F. ) ;
#2890 = ORIENTED_EDGE ( 'NONE', *, *, #19666, .F. ) ;
#2892 = EDGE_CURVE ( 'NONE', #12157, #8554, #13779, .T. ) ;
#2893 = DIRECTION ( 'NONE',  ( 0.01292394549866695240, 0.005513023399718316314, 0.9999012842304693116 ) ) ;
#2894 = EDGE_CURVE ( 'NONE', #18513, #3984, #17596, .T. ) ;
#2895 = CARTESIAN_POINT ( 'NONE',  ( -62.91398989571944611, 99.88146403284555674, 77.93815471138678674 ) ) ;
#2896 = DIRECTION ( 'NONE',  ( -0.009138748381789079875, -0.7071067811865487940, -0.7070477234798316912 ) ) ;
#2897 = DIRECTION ( 'NONE',  ( -0.01292394549866632963, -0.005513023399716958026, -0.9999012842304692006 ) ) ;
#2898 = CIRCLE ( 'NONE', #17962, 1.999999999999999778 ) ;
#2899 = FACE_OUTER_BOUND ( 'NONE', #5109, .T. ) ;
#2900 = CARTESIAN_POINT ( 'NONE',  ( -38.21549050681395698, 167.4026153394593734, 273.1339171915171846 ) ) ;
#2901 = ADVANCED_FACE ( 'NONE', ( #17215, #1487 ), #6756, .T. ) ;
#2902 = ORIENTED_EDGE ( 'NONE', *, *, #11528, .F. ) ;
#2903 = AXIS2_PLACEMENT_3D ( 'NONE', #8686, #5017, #3185 ) ;
#2904 = ORIENTED_EDGE ( 'NONE', *, *, #21545, .T. ) ;
#2905 = CARTESIAN_POINT ( 'NONE',  ( -46.79684245571608869, 129.3639651298425406, 248.1453739866443868 ) ) ;
#2906 = CARTESIAN_POINT ( 'NONE',  ( -49.99582398951010731, 170.0000000000000284, 0.6462070952320568828 ) ) ;
#2907 = CARTESIAN_POINT ( 'NONE',  ( 16.39634482804412130, 187.9401017119209882, 319.7988598509798521 ) ) ;
#2908 = CARTESIAN_POINT ( 'NONE',  ( -40.67014407421521582, 94.95224308429735061, 83.45134616373267988 ) ) ;
#2909 = CARTESIAN_POINT ( 'NONE',  ( -12.47967489686980613, 148.2895124671312317, 277.1262451100013777 ) ) ;
#2910 = ORIENTED_EDGE ( 'NONE', *, *, #794, .F. ) ;
#2911 =( NAMED_UNIT ( * ) SI_UNIT ( $, .STERADIAN. ) SOLID_ANGLE_UNIT ( ) );
#2912 = EDGE_CURVE ( 'NONE', #4443, #18526, #12890, .T. ) ;
#2913 = CARTESIAN_POINT ( 'NONE',  ( -49.22153082712133454, 106.9149828242082947, 60.55180848632685553 ) ) ;
#2914 = CARTESIAN_POINT ( 'NONE',  ( -64.01352119751047098, 100.1860183968354931, 76.74205626399758273 ) ) ;
#2915 = EDGE_LOOP ( 'NONE', ( #19963, #6877, #703, #3281 ) ) ;
#2916 = VERTEX_POINT ( 'NONE', #10442 ) ;
#2917 = AXIS2_PLACEMENT_3D ( 'NONE', #1580, #20400, #13867 ) ;
#2918 = ORIENTED_EDGE ( 'NONE', *, *, #10272, .F. ) ;
#2919 = CARTESIAN_POINT ( 'NONE',  ( -55.40268456415262932, 20.00000000000000000, 113.1659955246495883 ) ) ;
#2920 = AXIS2_PLACEMENT_3D ( 'NONE', #22344, #6190, #1484 ) ;
#2921 = ORIENTED_EDGE ( 'NONE', *, *, #4620, .T. ) ;
#2922 = LINE ( 'NONE', #884, #17279 ) ;
#2923 = LINE ( 'NONE', #22202, #8150 ) ;
#2924 = CARTESIAN_POINT ( 'NONE',  ( 84.18163614557413155, 75.11642389258673802, 3.622972191343602155 ) ) ;
#2925 = CARTESIAN_POINT ( 'NONE',  ( 0.000000000000000000, 0.000000000000000000, -78.99999999999998579 ) ) ;
#2926 = EDGE_CURVE ( 'NONE', #6314, #17705, #18678, .T. ) ;
#2927 = CARTESIAN_POINT ( 'NONE',  ( 17.62344600982285314, 187.4828202841882216, 275.9769641099970841 ) ) ;
#2928 = FACE_OUTER_BOUND ( 'NONE', #1579, .T. ) ;
#2929 = DIRECTION ( 'NONE',  ( 0.09199399308265900077, -0.9957502728239346901, 0.004301093787334644286 ) ) ;
#2930 = FACE_OUTER_BOUND ( 'NONE', #20042, .T. ) ;
#2931 = AXIS2_PLACEMENT_3D ( 'NONE', #12386, #12833, #12495 ) ;
#2932 = CONICAL_SURFACE ( 'NONE', #15799, 5.700000000000001954, 0.7853981633974482790 ) ;
#2933 = DIRECTION ( 'NONE',  ( -0.000000000000000000, -1.000000000000000000, -0.000000000000000000 ) ) ;
#2934 = CARTESIAN_POINT ( 'NONE',  ( 92.03665420188173130, 70.73625599351603910, 60.24390366714256118 ) ) ;
#2935 = EDGE_CURVE ( 'NONE', #14542, #9306, #20648, .T. ) ;
#2936 = ORIENTED_EDGE ( 'NONE', *, *, #19029, .T. ) ;
#2937 = DIRECTION ( 'NONE',  ( -7.125109674403838460E-05, 0.9999848031710254492, -0.005512562950847868688 ) ) ;
#2938 = AXIS2_PLACEMENT_3D ( 'NONE', #2626, #13203, #15166 ) ;
#2939 = DIRECTION ( 'NONE',  ( -0.7943823600057680068, 1.243025994321579861E-17, -0.6074180324222080429 ) ) ;
#2940 = ORIENTED_EDGE ( 'NONE', *, *, #11242, .T. ) ;
#2941 = DIRECTION ( 'NONE',  ( -2.025474946048326158E-22, 1.000000000000000000, -1.876735158486679638E-22 ) ) ;
#2942 = ORIENTED_EDGE ( 'NONE', *, *, #1657, .F. ) ;
#2943 = DIRECTION ( 'NONE',  ( 2.025474946048326158E-22, -1.000000000000000000, 1.876735158486679638E-22 ) ) ;
#2944 = AXIS2_PLACEMENT_3D ( 'NONE', #14138, #17819, #21116 ) ;
#2945 = AXIS2_PLACEMENT_3D ( 'NONE', #13181, #20145, #4417 ) ;
#2946 = CARTESIAN_POINT ( 'NONE',  ( -44.75576560912451640, 168.6025580852140706, 19.18675944895310082 ) ) ;
#2947 =( NAMED_UNIT ( * ) SI_UNIT ( $, .STERADIAN. ) SOLID_ANGLE_UNIT ( ) );
#2948 = CARTESIAN_POINT ( 'NONE',  ( 20.37582863626993301, 148.9655229296736820, 276.6108942144915659 ) ) ;
#2949 = EDGE_CURVE ( 'NONE', #11929, #20403, #4367, .T. ) ;
#2950 = AXIS2_PLACEMENT_3D ( 'NONE', #15940, #17886, #10862 ) ;
#2951 = EDGE_CURVE ( 'NONE', #12157, #19445, #4786, .T. ) ;
#2952 = CARTESIAN_POINT ( 'NONE',  ( 15.62064282387096092, 186.1419012809308526, 320.4776025279708733 ) ) ;
#2953 = ORIENTED_EDGE ( 'NONE', *, *, #19666, .T. ) ;
#2954 = CARTESIAN_POINT ( 'NONE',  ( 51.20005196345039167, 179.0478200177218184, 275.9143897845036122 ) ) ;
#2955 = VERTEX_POINT ( 'NONE', #5013 ) ;
#2956 = DIRECTION ( 'NONE',  ( 0.9999164797902017066, 6.965998958219365988E-18, -0.01292414190464157356 ) ) ;
#2957 = CARTESIAN_POINT ( 'NONE',  ( 9.142505149400571796, 70.80384757729338219, -88.65345271381767134 ) ) ;
#2958 = DIRECTION ( 'NONE',  ( 7.125109674081160920E-05, -0.9999848031710253382, 0.005512562950849312846 ) ) ;
#2959 = AXIS2_PLACEMENT_3D ( 'NONE', #9201, #11699, #17963 ) ;
#2960 = EDGE_LOOP ( 'NONE', ( #2054, #5081, #15427, #19986 ) ) ;
#2961 = CARTESIAN_POINT ( 'NONE',  ( 163.9999999999998863, 18.00000000000000355, 8.000000000002229328 ) ) ;
#2962 = AXIS2_PLACEMENT_3D ( 'NONE', #19575, #3850, #5332 ) ;
#2963 = ORIENTED_EDGE ( 'NONE', *, *, #5122, .F. ) ;
#2964 = CARTESIAN_POINT ( 'NONE',  ( 45.22160658036679592, 125.3750519639578727, 248.9782057516816849 ) ) ;
#2965 = CARTESIAN_POINT ( 'NONE',  ( -164.0000000000000000, 20.00000000000000000, 53.76161406891260697 ) ) ;
#2966 = AXIS2_PLACEMENT_3D ( 'NONE', #14015, #8695, #7325 ) ;
#2967 = DIRECTION ( 'NONE',  ( 0.01292414190464131335, 0.000000000000000000, 0.9999164797902017066 ) ) ;
#2968 = CARTESIAN_POINT ( 'NONE',  ( -146.5000000000000000, 1.999999999999998224, 8.000000000000017764 ) ) ;
#2969 = CARTESIAN_POINT ( 'NONE',  ( -28.54870338537778096, 324.0437177334164858, 313.3392609721734061 ) ) ;
#2970 = AXIS2_PLACEMENT_3D ( 'NONE', #16523, #4083, #11117 ) ;
#2971 = DIRECTION ( 'NONE',  ( -0.01292394549866740169, -0.005513023399721021615, -0.9999012842304692006 ) ) ;
#2972 = LINE ( 'NONE', #9987, #6926 ) ;
#2973 = DIRECTION ( 'NONE',  ( 0.9999164797902017066, 6.965998958219367529E-18, -0.01292414190464157182 ) ) ;
#2974 = PRODUCT_CONTEXT ( 'NONE', #20689, 'mechanical' ) ;
#2975 = EDGE_LOOP ( 'NONE', ( #4485, #13627 ) ) ;
#2976 = VECTOR ( 'NONE', #18954, 1000.000000000000227 ) ;
#2977 = CARTESIAN_POINT ( 'NONE',  ( -52.60896573992756942, 111.9218655255082524, -46.77848885693063608 ) ) ;
#2978 = ORIENTED_EDGE ( 'NONE', *, *, #20157, .F. ) ;
#2979 = DIRECTION ( 'NONE',  ( 0.01292394549866738782, 0.005513023399721131770, 0.9999012842304692006 ) ) ;
#2980 = LINE ( 'NONE', #17466, #21358 ) ;
#2981 = AXIS2_PLACEMENT_3D ( 'NONE', #1636, #15550, #15221 ) ;
#2982 = DIRECTION ( 'NONE',  ( -0.01292394549866731843, -0.005513023399720594006, -0.9999012842304693116 ) ) ;
#2983 = CARTESIAN_POINT ( 'NONE',  ( -8.562029719258356764, 342.2165115496170529, 328.2923693891043513 ) ) ;
#2984 = ORIENTED_EDGE ( 'NONE', *, *, #11262, .F. ) ;
#2985 = CARTESIAN_POINT ( 'NONE',  ( 34.90859880014114935, 93.86605675683669858, -83.28248650840920675 ) ) ;
#2986 = CIRCLE ( 'NONE', #20594, 8.000000000000003553 ) ;
#2987 = ORIENTED_EDGE ( 'NONE', *, *, #11212, .T. ) ;
#2988 = CARTESIAN_POINT ( 'NONE',  ( -50.56880203129856000, 139.7551263635817236, -43.68402316449832057 ) ) ;
#2989 = CARTESIAN_POINT ( 'NONE',  ( 106.2089377515399065, 72.00000000000000000, 28.62973177816241588 ) ) ;
#2990 = LINE ( 'NONE', #22262, #3376 ) ;
#2991 = DIRECTION ( 'NONE',  ( 0.9999164797902015955, 6.965998958219364448E-18, -0.01292414190464157182 ) ) ;
#2992 = SURFACE_STYLE_USAGE ( .BOTH. , #9679 ) ;
#2993 = AXIS2_PLACEMENT_3D ( 'NONE', #14151, #10570, #1728 ) ;
#2994 = ORIENTED_EDGE ( 'NONE', *, *, #12455, .F. ) ;
#2995 = AXIS2_PLACEMENT_3D ( 'NONE', #14715, #2633, #12992 ) ;
#2996 = DIRECTION ( 'NONE',  ( 0.9999164797902015955, 6.965998958219364448E-18, -0.01292414190464157182 ) ) ;
#2997 = DIRECTION ( 'NONE',  ( 0.9999164797902015955, 8.506845633049208051E-18, -0.01292414190464159611 ) ) ;
#2998 = ORIENTED_EDGE ( 'NONE', *, *, #8247, .F. ) ;
#2999 = AXIS2_PLACEMENT_3D ( 'NONE', #12428, #14512, #8849 ) ;
#3000 =( NAMED_UNIT ( * ) PLANE_ANGLE_UNIT ( ) SI_UNIT ( $, .RADIAN. ) );
#3001 = CARTESIAN_POINT ( 'NONE',  ( -90.10407258434753430, 87.47042737825177028, 51.11193766723834386 ) ) ;
#3002 = CIRCLE ( 'NONE', #2657, 7.000000000000022204 ) ;
#3004 = ORIENTED_EDGE ( 'NONE', *, *, #20722, .T. ) ;
#3003 = ORIENTED_EDGE ( 'NONE', *, *, #17644, .T. ) ;
#3005 = EDGE_CURVE ( 'NONE', #4814, #12132, #9983, .T. ) ;
#3006 = CARTESIAN_POINT ( 'NONE',  ( -74.75841872729287729, 95.60624342341641579, 80.69196661707292151 ) ) ;
#3007 = DIRECTION ( 'NONE',  ( 0.01292394549866743812, 0.005513023399720639109, 0.9999012842304693116 ) ) ;
#3008 = FACE_OUTER_BOUND ( 'NONE', #10174, .T. ) ;
#3009 = ORIENTED_EDGE ( 'NONE', *, *, #20733, .T. ) ;
#3010 = DIRECTION ( 'NONE',  ( 0.9999164797902015955, 2.001050586450178695E-22, -0.01292414190464131335 ) ) ;
#3011 = EDGE_CURVE ( 'NONE', #14045, #1288, #12477, .T. ) ;
#3012 = CARTESIAN_POINT ( 'NONE',  ( -92.19968689859017275, 79.04398536104956463, 28.61667231988787563 ) ) ;
#3013 = AXIS2_PLACEMENT_3D ( 'NONE', #8562, #5101, #10300 ) ;
#3014 = AXIS2_PLACEMENT_3D ( 'NONE', #645, #9128, #16179 ) ;
#3015 = DIRECTION ( 'NONE',  ( 0.009760756503428048153, -0.9999378516499565217, 0.005387065077612505741 ) ) ;
#3016 = ORIENTED_EDGE ( 'NONE', *, *, #743, .F. ) ;
#3017 = EDGE_CURVE ( 'NONE', #555, #4443, #6639, .T. ) ;
#3018 = CARTESIAN_POINT ( 'NONE',  ( 1.364374644014609697E-14, 69.99999999999998579, -9.836443712999143722E-15 ) ) ;
#3019 = CARTESIAN_POINT ( 'NONE',  ( -20.57109388430227881, 136.7551719540686008, -44.05520973278501629 ) ) ;
#3020 = CARTESIAN_POINT ( 'NONE',  ( 16.40873467034967703, 185.6567299720570645, 322.3321779654822876 ) ) ;
#3021 = DIRECTION ( 'NONE',  ( 0.01292394549868127775, 0.005513023399721131770, 0.9999012842304690896 ) ) ;
#3022 = FACE_OUTER_BOUND ( 'NONE', #68, .T. ) ;
#3023 = ORIENTED_EDGE ( 'NONE', *, *, #19180, .F. ) ;
#3024 = DIRECTION ( 'NONE',  ( 0.000000000000000000, 0.000000000000000000, 1.000000000000000000 ) ) ;
#3025 = ADVANCED_FACE ( 'NONE', ( #21100 ), #10886, .T. ) ;
#3026 = EDGE_CURVE ( 'NONE', #10108, #11275, #11366, .T. ) ;
#3027 = CARTESIAN_POINT ( 'NONE',  ( -12.58664483627419095, 184.6272112293399630, 320.1917372557430213 ) ) ;
#3028 = EDGE_CURVE ( 'NONE', #10034, #2793, #9147, .T. ) ;
#3029 = EDGE_LOOP ( 'NONE', ( #20083, #8455, #1204, #1954 ) ) ;
#3031 = CARTESIAN_POINT ( 'NONE',  ( -7.355408695361009386, 188.2724542843479867, 276.2720482804903099 ) ) ;
#3030 = VECTOR ( 'NONE', #19503, 1000.000000000000000 ) ;
#3032 = ORIENTED_EDGE ( 'NONE', *, *, #13991, .T. ) ;
#3033 = AXIS2_PLACEMENT_3D ( 'NONE', #18081, #2551, #12782 ) ;
#3034 = CARTESIAN_POINT ( 'NONE',  ( -0.9693106428480922077, 69.99999999999998579, -74.99373598426512899 ) ) ;
#3035 = ADVANCED_FACE ( 'NONE', ( #3639 ), #6855, .T. ) ;
#3036 = ORIENTED_EDGE ( 'NONE', *, *, #5413, .T. ) ;
#3037 =( LENGTH_UNIT ( ) NAMED_UNIT ( * ) SI_UNIT ( .MILLI., .METRE. ) );
#3038 = DIRECTION ( 'NONE',  ( 0.009371490965938892789, 0.6886276452575282869, 0.7250545781830131098 ) ) ;
#3039 = EDGE_CURVE ( 'NONE', #10639, #11300, #2073, .T. ) ;
#3040 = EDGE_CURVE ( 'NONE', #495, #6274, #5477, .T. ) ;
#3041 = CARTESIAN_POINT ( 'NONE',  ( 105.4334892372614405, 77.12912189496645965, -31.36525700924962834 ) ) ;
#3042 = FACE_OUTER_BOUND ( 'NONE', #12897, .T. ) ;
#3043 = ADVANCED_FACE ( 'NONE', ( #13999 ), #21605, .T. ) ;
#3044 = CARTESIAN_POINT ( 'NONE',  ( 15.34924354053137741, 187.7676347092321407, 277.1267350366562709 ) ) ;
#3045 = DIRECTION ( 'NONE',  ( 0.3101392564284313202, 0.9506461370142480494, -0.009250070373107143265 ) ) ;
#3046 = DIRECTION ( 'NONE',  ( 0.9999164797902015955, 6.965998958219364448E-18, -0.01292414190464157182 ) ) ;
#3047 = CARTESIAN_POINT ( 'NONE',  ( -44.75576560912451640, 168.6025580852140706, 19.18675944895310082 ) ) ;
#3048 = AXIS2_PLACEMENT_3D ( 'NONE', #15582, #22532, #4864 ) ;
#3049 = DIRECTION ( 'NONE',  ( 0.9999164797902015955, 0.000000000000000000, -0.01292414190463754553 ) ) ;
#3050 = EDGE_CURVE ( 'NONE', #13705, #9861, #5097, .T. ) ;
#3051 = CIRCLE ( 'NONE', #21734, 95.00000000000001421 ) ;
#3052 = DIRECTION ( 'NONE',  ( 7.125109674403276030E-05, -0.9999848031710252272, 0.005512562950848280685 ) ) ;
#3053 = CARTESIAN_POINT ( 'NONE',  ( -39.48280323120003032, 107.3915498679189682, 71.96693194386834591 ) ) ;
#3054 = VERTEX_POINT ( 'NONE', #19146 ) ;
#3055 = ADVANCED_FACE ( 'NONE', ( #3421 ), #10543, .F. ) ;
#3056 = ORIENTED_EDGE ( 'NONE', *, *, #13781, .T. ) ;
#3057 = CARTESIAN_POINT ( 'NONE',  ( -11.14887313374392264, 155.5756827379013885, 104.6149162130246140 ) ) ;
#3058 = DIRECTION ( 'NONE',  ( 0.01292394549866738955, 0.005513023399720468239, 0.9999012842304693116 ) ) ;
#3059 = ORIENTED_EDGE ( 'NONE', *, *, #13281, .F. ) ;
#3060 = AXIS2_PLACEMENT_3D ( 'NONE', #3257, #9946, #9831 ) ;
#3061 = EDGE_CURVE ( 'NONE', #13946, #3588, #8681, .T. ) ;
#3062 = CARTESIAN_POINT ( 'NONE',  ( 7.319796769195226815, 70.14698466122824527, -86.26971152178253988 ) ) ;
#3063 = VERTEX_POINT ( 'NONE', #9028 ) ;
#3064 = ADVANCED_FACE ( 'NONE', ( #19265 ), #4587, .T. ) ;
#3065 = AXIS2_PLACEMENT_3D ( 'NONE', #6930, #3841, #7054 ) ;
#3066 = VECTOR ( 'NONE', #8424, 999.9999999999998863 ) ;
#3067 = CARTESIAN_POINT ( 'NONE',  ( -68.01573619543681559, 70.58429683895616336, 86.45204278734176739 ) ) ;
#3068 = CARTESIAN_POINT ( 'NONE',  ( -6.532353581617583060, 165.6256992825491068, 113.6007336314425231 ) ) ;
#3069 = CARTESIAN_POINT ( 'NONE',  ( 39.43544423852503655, 124.9314917220301737, -43.93710795200372843 ) ) ;
#3070 = EDGE_CURVE ( 'NONE', #6117, #7048, #2074, .T. ) ;
#3071 = DIRECTION ( 'NONE',  ( -0.01292394549866745720, -0.005513023399720816918, -0.9999012842304692006 ) ) ;
#3072 = CIRCLE ( 'NONE', #4542, 1.999999999999998224 ) ;
#3073 = DIRECTION ( 'NONE',  ( 0.9999164797902015955, 2.045733645417851681E-15, -0.01292414190464156835 ) ) ;
#3074 = ORIENTED_EDGE ( 'NONE', *, *, #22228, .T. ) ;
#3075 = FACE_OUTER_BOUND ( 'NONE', #4265, .T. ) ;
#3076 = CARTESIAN_POINT ( 'NONE',  ( 7.145902869757795983, 69.99999999999998579, -93.45069977196735067 ) ) ;
#3077 = AXIS2_PLACEMENT_3D ( 'NONE', #16306, #5582, #16188 ) ;
#3078 = ORIENTED_EDGE ( 'NONE', *, *, #5726, .F. ) ;
#3079 = CARTESIAN_POINT ( 'NONE',  ( 4.169604791867612015, 166.7785703876306513, 322.5944574396354483 ) ) ;
#3080 = VECTOR ( 'NONE', #1739, 1000.000000000000000 ) ;
#3081 = ORIENTED_EDGE ( 'NONE', *, *, #15743, .F. ) ;
#3082 = CARTESIAN_POINT ( 'NONE',  ( 86.02081024124220221, 103.0873963570200118, -68.57787521732684866 ) ) ;
#3083 = CARTESIAN_POINT ( 'NONE',  ( 50.91257692374890809, 106.8061942917681790, 70.28123811582710800 ) ) ;
#3084 = APPLICATION_CONTEXT ( 'automotive_design' ) ;
#3085 = CARTESIAN_POINT ( 'NONE',  ( 0.000000000000000000, 45.00000000000000711, -83.99999999999998579 ) ) ;
#3086 = EDGE_CURVE ( 'NONE', #16183, #20403, #17837, .T. ) ;
#3087 = CIRCLE ( 'NONE', #13400, 22.49999999999999645 ) ;
#3088 = LINE ( 'NONE', #13551, #19969 ) ;
#3089 = ITEM_DEFINED_TRANSFORMATION ( 'NONE', 'NONE', #8845,  #6292 ) ;
#3090 = CIRCLE ( 'NONE', #6760, 22.40787840283382693 ) ;
#3091 = EDGE_LOOP ( 'NONE', ( #13209, #20791, #10498, #3830 ) ) ;
#3092 = CIRCLE ( 'NONE', #16332, 11.00000000000000178 ) ;
#3093 = DIRECTION ( 'NONE',  ( 0.9999164797902015955, 2.457859219970326020E-15, -0.01292414190464043211 ) ) ;
#3094 = DIRECTION ( 'NONE',  ( -0.01292394549866738782, -0.005513023399720468239, -0.9999012842304692006 ) ) ;
#3095 = DIRECTION ( 'NONE',  ( -0.01292394549866754394, -0.005513023399720772683, -0.9999012842304692006 ) ) ;
#3096 = FACE_OUTER_BOUND ( 'NONE', #16126, .T. ) ;
#3097 = DIRECTION ( 'NONE',  ( 7.125109674161246868E-05, -0.9999848031710252272, 0.005512562950850154186 ) ) ;
#3098 = CARTESIAN_POINT ( 'NONE',  ( 92.40872671617952960, 34.61572286322119396, -33.19707612406970298 ) ) ;
#3099 = VERTEX_POINT ( 'NONE', #5046 ) ;
#3100 = CARTESIAN_POINT ( 'NONE',  ( -89.76989948563728205, 88.05754991457587266, 50.75033462167537834 ) ) ;
#3101 = ORIENTED_EDGE ( 'NONE', *, *, #20324, .F. ) ;
#3102 = CARTESIAN_POINT ( 'NONE',  ( 0.000000000000000000, 0.000000000000000000, 0.000000000000000000 ) ) ;
#3103 = CARTESIAN_POINT ( 'NONE',  ( -91.21019055468684655, 72.00000000000000000, -28.82359390673209631 ) ) ;
#3104 = CIRCLE ( 'NONE', #14882, 10.29295143883735619 ) ;
#3105 = CARTESIAN_POINT ( 'NONE',  ( 45.73105848731719192, 168.8134312302534283, 56.26981079935081453 ) ) ;
#3106 = FACE_OUTER_BOUND ( 'NONE', #10728, .T. ) ;
#3107 = ORIENTED_EDGE ( 'NONE', *, *, #9033, .F. ) ;
#3108 = PLANE ( 'NONE',  #20633 ) ;
#3109 = CARTESIAN_POINT ( 'NONE',  ( -51.82743751170760049, 114.6914167488026095, 172.2189919798578899 ) ) ;
#3110 = ORIENTED_EDGE ( 'NONE', *, *, #12999, .T. ) ;
#3111 = DIRECTION ( 'NONE',  ( -0.9999164797902015955, 0.000000000000000000, 0.01292414190464162733 ) ) ;
#3112 = EDGE_CURVE ( 'NONE', #5442, #4756, #8820, .T. ) ;
#3113 = DIRECTION ( 'NONE',  ( 0.000000000000000000, 0.000000000000000000, 1.000000000000000000 ) ) ;
#3114 = EDGE_CURVE ( 'NONE', #9573, #4798, #14502, .T. ) ;
#3115 = ORIENTED_EDGE ( 'NONE', *, *, #7712, .T. ) ;
#3116 = DIRECTION ( 'NONE',  ( -0.009985269297354625040, -0.6348858185549794975, -0.7725414498878574454 ) ) ;
#3117 = CARTESIAN_POINT ( 'NONE',  ( -90.11629072746302427, 87.42992512273923467, 51.13668368328682590 ) ) ;
#3118 = STYLED_ITEM ( 'NONE', ( #21133 ), #9964 ) ;
#3120 = VERTEX_POINT ( 'NONE', #14725 ) ;
#3119 = EDGE_LOOP ( 'NONE', ( #3878, #1092, #5398, #5843 ) ) ;
#3121 = CARTESIAN_POINT ( 'NONE',  ( -11.47153213676876859, 182.9699874009099858, 322.8803889165183136 ) ) ;
#3122 = CARTESIAN_POINT ( 'NONE',  ( -34.90911429189236515, 93.86615990965727008, 83.28258796055321511 ) ) ;
#3123 = CARTESIAN_POINT ( 'NONE',  ( 394.6585245357460963, 69.99999999999997158, -112.1099862245463896 ) ) ;
#3124 = EDGE_LOOP ( 'NONE', ( #3780, #13835, #15612, #7870 ) ) ;
#3125 = CARTESIAN_POINT ( 'NONE',  ( 50.24995405803858262, 113.2674379272951910, -44.84108624765922713 ) ) ;
#3126 = PRODUCT_RELATED_PRODUCT_CATEGORY ( 'part', '', ( #16046 ) ) ;
#3127 = CARTESIAN_POINT ( 'NONE',  ( -51.86045928498519686, 189.4905222308084660, -91.80463846584517285 ) ) ;
#3128 = ORIENTED_EDGE ( 'NONE', *, *, #1349, .F. ) ;
#3129 = ORIENTED_EDGE ( 'NONE', *, *, #22301, .F. ) ;
#3130 = LINE ( 'NONE', #9808, #9170 ) ;
#3131 = CARTESIAN_POINT ( 'NONE',  ( -44.04984536558698238, 154.0021226047651908, 277.2836069455634060 ) ) ;
#3132 = DIRECTION ( 'NONE',  ( 0.01292394549866738782, 0.005513023399720700692, 0.9999012842304693116 ) ) ;
#3133 = DIRECTION ( 'NONE',  ( 0.01292414190464131335, 1.902755938799530239E-22, 0.9999164797902015955 ) ) ;
#3134 = CARTESIAN_POINT ( 'NONE',  ( -70.88807251563926570, 91.17157287525390075, -82.09068872300603914 ) ) ;
#3135 =( NAMED_UNIT ( * ) SI_UNIT ( $, .STERADIAN. ) SOLID_ANGLE_UNIT ( ) );
#3136 = CARTESIAN_POINT ( 'NONE',  ( -38.46706438352712354, 72.00000000000000000, 85.27439087629284131 ) ) ;
#3137 = SHAPE_REPRESENTATION ( 'Jaw', ( #6292 ), #1540 ) ;
#3138 = AXIS2_PLACEMENT_3D ( 'NONE', #15898, #10250, #12331 ) ;
#3139 = CARTESIAN_POINT ( 'NONE',  ( -10.34796365319335543, 187.1999046744221857, 321.1016630495802815 ) ) ;
#3140 = ORIENTED_EDGE ( 'NONE', *, *, #20593, .T. ) ;
#3141 = EDGE_CURVE ( 'NONE', #18838, #9416, #12211, .T. ) ;
#3142 = ORIENTED_EDGE ( 'NONE', *, *, #1210, .T. ) ;
#3143 = CARTESIAN_POINT ( 'NONE',  ( 3.872354045398203937, 166.6517708494369856, 299.5967279023338392 ) ) ;
#3144 = ORIENTED_EDGE ( 'NONE', *, *, #4857, .F. ) ;
#3145 = CARTESIAN_POINT ( 'NONE',  ( -49.34917620029669649, 107.4660479794951584, 70.81942874090999851 ) ) ;
#3146 = CARTESIAN_POINT ( 'NONE',  ( -88.05170339851980543, 72.97786998644572520, 61.56719313945617245 ) ) ;
#3147 = VECTOR ( 'NONE', #4925, 1000.000000000000000 ) ;
#3148 = CARTESIAN_POINT ( 'NONE',  ( -146.5000000000000000, 18.00000000000000355, 2.081668171172168513E-14 ) ) ;
#3149 = EDGE_CURVE ( 'NONE', #10602, #22152, #21465, .T. ) ;
#3150 = CARTESIAN_POINT ( 'NONE',  ( 79.99331838321626265, 102.0000000000000000, -1.033931352371318058 ) ) ;
#3151 = DIRECTION ( 'NONE',  ( 0.9232306267972780756, 0.000000000000000000, -0.3842462878721211728 ) ) ;
#3152 = CARTESIAN_POINT ( 'NONE',  ( 1.445083222993876641E-14, 23.00000000000000000, -118.0000000000000000 ) ) ;
#3153 = CARTESIAN_POINT ( 'NONE',  ( -90.00000000000000000, 45.00100000000000477, 10.99999999999999289 ) ) ;
#3154 = DIRECTION ( 'NONE',  ( -0.9999164797902015955, 0.000000000000000000, 0.01292414190464162733 ) ) ;
#3155 = CARTESIAN_POINT ( 'NONE',  ( -52.66211423087264620, 189.6011917897851333, -71.71870077557677803 ) ) ;
#3156 = CARTESIAN_POINT ( 'NONE',  ( 90.41053243085600855, 78.34173690304720594, -33.04444670410838825 ) ) ;
#3157 = ORIENTED_EDGE ( 'NONE', *, *, #9476, .F. ) ;
#3158 = LINE ( 'NONE', #4757, #9574 ) ;
#3159 = CARTESIAN_POINT ( 'NONE',  ( -10.05250806467569546, 187.8426943151429498, 308.1634901438939664 ) ) ;
#3160 = ORIENTED_EDGE ( 'NONE', *, *, #8301, .F. ) ;
#3161 = DIRECTION ( 'NONE',  ( 0.9999164797902015955, -8.863511990578706951E-16, -0.01292414190464158050 ) ) ;
#3162 = EDGE_CURVE ( 'NONE', #17867, #12773, #9174, .T. ) ;
#3163 = VERTEX_POINT ( 'NONE', #16345 ) ;
#3164 = EDGE_CURVE ( 'NONE', #13257, #15597, #21565, .T. ) ;
#3165 = CARTESIAN_POINT ( 'NONE',  ( -67.13053572995303853, 70.13637825286163263, 87.14080137989778052 ) ) ;
#3166 = CARTESIAN_POINT ( 'NONE',  ( -4.006862498311197562, 172.5094284590153393, 324.6687400670222701 ) ) ;
#3167 = CARTESIAN_POINT ( 'NONE',  ( 70.90635001240286783, 92.58578643762697880, 83.50478416996566011 ) ) ;
#3168 = EDGE_CURVE ( 'NONE', #11414, #11720, #12870, .T. ) ;
#3169 = CARTESIAN_POINT ( 'NONE',  ( 18.74581175270508027, 147.5432771199994875, 276.8255568971947582 ) ) ;
#3170 = VERTEX_POINT ( 'NONE', #3999 ) ;
#3171 = CARTESIAN_POINT ( 'NONE',  ( -39.40254987707573520, 92.58578643762697880, 84.93055112583743949 ) ) ;
#3172 = EDGE_CURVE ( 'NONE', #12249, #8826, #8048, .T. ) ;
#3173 = CARTESIAN_POINT ( 'NONE',  ( 106.9749367633763910, 78.91761970611439381, 25.61958048976759983 ) ) ;
#3174 = ORIENTED_EDGE ( 'NONE', *, *, #22256, .F. ) ;
#3175 = FILL_AREA_STYLE_COLOUR ( '', #14775 ) ;
#3176 = VERTEX_POINT ( 'NONE', #2418 ) ;
#3177 = CARTESIAN_POINT ( 'NONE',  ( 21.74583478316889185, 185.4784524348809782, 278.2598337873663468 ) ) ;
#3178 = DIRECTION ( 'NONE',  ( 0.000000000000000000, 0.000000000000000000, -1.000000000000000000 ) ) ;
#3179 = DIRECTION ( 'NONE',  ( -0.9999164797902015955, -6.965998958219364448E-18, 0.01292414190464157182 ) ) ;
#3180 = DIRECTION ( 'NONE',  ( -1.000000000000000000, 0.000000000000000000, -1.362186893977296347E-14 ) ) ;
#3181 = ADVANCED_FACE ( 'NONE', ( #19629 ), #11024, .T. ) ;
#3182 = CARTESIAN_POINT ( 'NONE',  ( -44.54898248114630377, 168.6907664596094776, 35.18517999664061335 ) ) ;
#3183 = ORIENTED_EDGE ( 'NONE', *, *, #20658, .T. ) ;
#3184 = EDGE_CURVE ( 'NONE', #22618, #21849, #21353, .T. ) ;
#3185 = DIRECTION ( 'NONE',  ( -0.2317097747526812579, 0.9727820773532223075, -0.002368599673008277024 ) ) ;
#3186 = AXIS2_PLACEMENT_3D ( 'NONE', #4220, #14597, #11136 ) ;
#3187 = DIRECTION ( 'NONE',  ( 0.01292394549866695240, 0.005513023399718316314, 0.9999012842304693116 ) ) ;
#3188 = ITEM_DEFINED_TRANSFORMATION ( 'NONE', 'NONE', #1132,  #6292 ) ;
#3189 = ORIENTED_EDGE ( 'NONE', *, *, #18250, .F. ) ;
#3190 = LINE ( 'NONE', #10447, #3750 ) ;
#3191 = CARTESIAN_POINT ( 'NONE',  ( -55.40268456415265774, 18.00000000000000355, -113.1659955246495741 ) ) ;
#3192 = CARTESIAN_POINT ( 'NONE',  ( -64.07781940414963628, 106.8060942374655156, 71.76742530483514315 ) ) ;
#3193 = CARTESIAN_POINT ( 'NONE',  ( -1.163172771417702700, 37.00000000000000711, -89.99248318111824574 ) ) ;
#3194 = VERTEX_POINT ( 'NONE', #7686 ) ;
#3195 = CARTESIAN_POINT ( 'NONE',  ( -56.89103422957282419, 143.2573102595449654, 47.48611753646095224 ) ) ;
#3196 = CARTESIAN_POINT ( 'NONE',  ( -1.386679829960242619E-13, 20.00000000000000000, -9.999999999999994671 ) ) ;
#3197 = ORIENTED_EDGE ( 'NONE', *, *, #16325, .T. ) ;
#3198 = EDGE_CURVE ( 'NONE', #21215, #530, #19771, .T. ) ;
#3199 = CARTESIAN_POINT ( 'NONE',  ( -88.71179014270776975, 88.67509488062695766, 50.35684176716525684 ) ) ;
#3200 = ORIENTED_EDGE ( 'NONE', *, *, #19412, .F. ) ;
#3201 =( NAMED_UNIT ( * ) PLANE_ANGLE_UNIT ( ) SI_UNIT ( $, .RADIAN. ) );
#3202 = CARTESIAN_POINT ( 'NONE',  ( -11.46885069223597853, 70.80384757729338219, -91.33151364841882014 ) ) ;
#3203 = FACE_OUTER_BOUND ( 'NONE', #2686, .T. ) ;
#3204 = CARTESIAN_POINT ( 'NONE',  ( 53.21979840114054383, 141.3748088146942621, 248.7866116092309881 ) ) ;
#3205 = CIRCLE ( 'NONE', #2855, 22.50000000000000000 ) ;
#3206 = ORIENTED_EDGE ( 'NONE', *, *, #18469, .T. ) ;
#3207 = DIRECTION ( 'NONE',  ( 0.9999164797902017066, -7.828075210616901716E-16, -0.01292414190464158050 ) ) ;
#3208 = FILL_AREA_STYLE_COLOUR ( '', #4212 ) ;
#3209 = VECTOR ( 'NONE', #7295, 1000.000000000000114 ) ;
#3210 = ORIENTED_EDGE ( 'NONE', *, *, #9343, .T. ) ;
#3211 = EDGE_CURVE ( 'NONE', #5755, #8095, #4433, .T. ) ;
#3212 = CARTESIAN_POINT ( 'NONE',  ( 14.14167086503323034, 113.6998737626107641, 126.9321988120954643 ) ) ;
#3213 = ORIENTED_EDGE ( 'NONE', *, *, #22107, .T. ) ;
#3214 = AXIS2_PLACEMENT_3D ( 'NONE', #20557, #18848, #3111 ) ;
#3215 = CARTESIAN_POINT ( 'NONE',  ( 91.02819465875460025, 70.25795030837511490, -61.75749006523108164 ) ) ;
#3216 = CARTESIAN_POINT ( 'NONE',  ( -90.02893273579236677, 88.66443490277293904, 52.56386379439879875 ) ) ;
#3218 = VERTEX_POINT ( 'NONE', #12658 ) ;
#3217 = ORIENTED_EDGE ( 'NONE', *, *, #1523, .F. ) ;
#3219 = VERTEX_POINT ( 'NONE', #18265 ) ;
#3220 = CARTESIAN_POINT ( 'NONE',  ( -75.17435380461473926, 95.13881385111719169, 80.30459320758008346 ) ) ;
#3221 = LINE ( 'NONE', #5055, #9631 ) ;
#3222 = CARTESIAN_POINT ( 'NONE',  ( -51.96670106358950392, 114.1985000165065429, 163.8168499024120592 ) ) ;
#3223 = FILL_AREA_STYLE_COLOUR ( '', #5839 ) ;
#3224 = CARTESIAN_POINT ( 'NONE',  ( 146.4999999999998579, 20.00000000000000000, -10.00000000000202682 ) ) ;
#3225 = DIRECTION ( 'NONE',  ( 0.7944560844389294552, 0.000000000000000000, 0.6073216033519345247 ) ) ;
#3226 = ORIENTED_EDGE ( 'NONE', *, *, #3870, .F. ) ;
#3227 = EDGE_CURVE ( 'NONE', #17055, #3176, #6371, .T. ) ;
#3228 = ORIENTED_EDGE ( 'NONE', *, *, #13506, .F. ) ;
#3229 = ADVANCED_FACE ( 'NONE', ( #17210 ), #13216, .F. ) ;
#3230 = DIRECTION ( 'NONE',  ( 0.9999164797902017066, 6.965998958219365988E-18, -0.01292414190464157356 ) ) ;
#3231 = DIRECTION ( 'NONE',  ( 0.01096700916508639573, -0.5290868411612598132, 0.8484968115555726609 ) ) ;
#3232 = DIRECTION ( 'NONE',  ( 0.009760756503427813965, -0.9999378516499565217, 0.005387065077607405654 ) ) ;
#3233 = AXIS2_PLACEMENT_3D ( 'NONE', #17889, #9120, #2123 ) ;
#3234 = CARTESIAN_POINT ( 'NONE',  ( -5.380602081949200866, 174.4012639950344976, 324.6760651920582745 ) ) ;
#3235 = CARTESIAN_POINT ( 'NONE',  ( -8.910000229846922082, 145.6729472732380088, 276.9535057578845567 ) ) ;
#3236 = AXIS2_PLACEMENT_3D ( 'NONE', #9475, #20038, #9606 ) ;
#3237 = CARTESIAN_POINT ( 'NONE',  ( 44.91100620407951993, 166.8507685304810764, 256.0609518519894436 ) ) ;
#3238 = AXIS2_PLACEMENT_3D ( 'NONE', #10361, #17370, #21138 ) ;
#3239 =( REPRESENTATION_RELATIONSHIP ('NONE','NONE', #11808, #15770 ) REPRESENTATION_RELATIONSHIP_WITH_TRANSFORMATION ( #7102 )SHAPE_REPRESENTATION_RELATIONSHIP( ) );
#3240 = CARTESIAN_POINT ( 'NONE',  ( 3.808636396294353688, 166.6245905359224082, 294.6670135843256162 ) ) ;
#3241 = ORIENTED_EDGE ( 'NONE', *, *, #9392, .F. ) ;
#3242 = ORIENTED_EDGE ( 'NONE', *, *, #6069, .T. ) ;
#3243 = VERTEX_POINT ( 'NONE', #18490 ) ;
#3244 = CARTESIAN_POINT ( 'NONE',  ( -90.04240250630805065, 70.00863645477431874, 63.19825073092409440 ) ) ;
#3245 = VECTOR ( 'NONE', #11608, 1000.000000000000000 ) ;
#3247 = VERTEX_POINT ( 'NONE', #8021 ) ;
#3246 = ORIENTED_EDGE ( 'NONE', *, *, #6278, .F. ) ;
#3248 = CARTESIAN_POINT ( 'NONE',  ( -49.09967157776827662, 108.0238286078847523, 69.97982874036236467 ) ) ;
#3249 = CARTESIAN_POINT ( 'NONE',  ( -90.16402721638407058, 71.32383232314188604, 60.62233968236869686 ) ) ;
#3250 = CIRCLE ( 'NONE', #12059, 2.000000000000001332 ) ;
#3251 = CARTESIAN_POINT ( 'NONE',  ( 50.79397376011281295, 189.4876967392748384, -93.64401692289283119 ) ) ;
#3252 = EDGE_CURVE ( 'NONE', #15219, #6364, #20313, .T. ) ;
#3253 = CARTESIAN_POINT ( 'NONE',  ( -49.99582398951010731, 170.0000000000000284, 0.6462070952320568828 ) ) ;
#3254 = VERTEX_POINT ( 'NONE', #11599 ) ;
#3255 = DIRECTION ( 'NONE',  ( -0.003413786507416180071, 0.9644842718275419280, -0.2641182225045783927 ) ) ;
#3256 = FACE_OUTER_BOUND ( 'NONE', #22115, .T. ) ;
#3257 = CARTESIAN_POINT ( 'NONE',  ( 91.62437796271727564, 34.61572286322119396, 60.86849236629024773 ) ) ;
#3258 = CARTESIAN_POINT ( 'NONE',  ( 51.07319921393754214, 94.45452722259994971, 82.70828171889884572 ) ) ;
#3259 = CARTESIAN_POINT ( 'NONE',  ( 79.99331838321626265, 55.99999999999999289, -7.033931352371318724 ) ) ;
#3260 = ORIENTED_EDGE ( 'NONE', *, *, #20639, .F. ) ;
#3261 = CARTESIAN_POINT ( 'NONE',  ( 79.99331838321614896, 55.00000000000000000, -1.033931352371314949 ) ) ;
#3262 = CLOSED_SHELL ( 'NONE', ( #960, #13040, #16685, #12758, #12715, #2611, #14277, #3229, #16518, #17138, #11889, #12219, #12513, #10902, #16471, #20249 ) ) ;
#3263 = AXIS2_PLACEMENT_3D ( 'NONE', #14223, #7422, #21199 ) ;
#3264 = DIRECTION ( 'NONE',  ( 0.01292414190464131335, 1.902755938799530239E-22, 0.9999164797902015955 ) ) ;
#3265 = DIRECTION ( 'NONE',  ( -2.025474946048326158E-22, 1.000000000000000000, -1.876735158486679638E-22 ) ) ;
#3266 = AXIS2_PLACEMENT_3D ( 'NONE', #930, #22242, #11707 ) ;
#3267 = ORIENTED_EDGE ( 'NONE', *, *, #818, .T. ) ;
#3268 = CARTESIAN_POINT ( 'NONE',  ( -91.26841073957253059, 80.27011201452100408, -30.02500290034050323 ) ) ;
#3269 = ORIENTED_EDGE ( 'NONE', *, *, #6493, .F. ) ;
#3270 = CARTESIAN_POINT ( 'NONE',  ( -70.91392079944854743, 91.17157287525390075, -84.09052168258642723 ) ) ;
#3271 = PRODUCT_DEFINITION_CONTEXT ( 'detailed design', #8949, 'design' ) ;
#3272 = VECTOR ( 'NONE', #9548, 1000.000000000000227 ) ;
#3273 = EDGE_CURVE ( 'NONE', #11778, #4144, #1151, .T. ) ;
#3274 = CARTESIAN_POINT ( 'NONE',  ( 44.03052579490771024, 164.6879759653328961, -75.29719582347730977 ) ) ;
#3275 =( GEOMETRIC_REPRESENTATION_CONTEXT ( 3 ) GLOBAL_UNCERTAINTY_ASSIGNED_CONTEXT ( ( #20316 ) ) GLOBAL_UNIT_ASSIGNED_CONTEXT ( ( #12330, #3354, #22394 ) ) REPRESENTATION_CONTEXT ( 'NONE', 'WORKASPACE' ) );
#3276 = CARTESIAN_POINT ( 'NONE',  ( 0.000000000000000000, 25.00000000000000000, -120.0000000000000000 ) ) ;
#3277 = CARTESIAN_POINT ( 'NONE',  ( 10.25516029832731846, 143.0782243734045949, 275.1688085660350680 ) ) ;
#3278 = ORIENTED_EDGE ( 'NONE', *, *, #22435, .F. ) ;
#3279 = VECTOR ( 'NONE', #12398, 1000.000000000000227 ) ;
#3280 = CARTESIAN_POINT ( 'NONE',  ( 13.24628194959730010, 190.1869353459286174, 320.8311507295203455 ) ) ;
#3281 = ORIENTED_EDGE ( 'NONE', *, *, #13013, .T. ) ;
#3282 = DIRECTION ( 'NONE',  ( 0.9999164797902017066, 2.001050586450178931E-22, -0.01292414190464131508 ) ) ;
#3283 = EDGE_CURVE ( 'NONE', #1879, #2134, #2566, .T. ) ;
#3284 = CARTESIAN_POINT ( 'NONE',  ( 108.6468492096305596, 76.31988324137756763, -17.34982836191095146 ) ) ;
#3285 = ORIENTED_EDGE ( 'NONE', *, *, #2807, .F. ) ;
#3286 = CARTESIAN_POINT ( 'NONE',  ( 108.7507233931858082, 76.71731347669783929, 17.16766896971239120 ) ) ;
#3287 = CIRCLE ( 'NONE', #16542, 2.009999999999995346 ) ;
#3288 = DIRECTION ( 'NONE',  ( 0.000000000000000000, 1.000000000000000000, -0.000000000000000000 ) ) ;
#3289 = ORIENTED_EDGE ( 'NONE', *, *, #5069, .F. ) ;
#3290 = CARTESIAN_POINT ( 'NONE',  ( -66.54881943730367766, 192.1904093341287307, 35.33996588919776372 ) ) ;
#3291 = ORIENTED_EDGE ( 'NONE', *, *, #17774, .T. ) ;
#3292 = DIRECTION ( 'NONE',  ( -0.9935244165829104634, -0.1136188085379686713, 0.000000000000000000 ) ) ;
#3293 = CARTESIAN_POINT ( 'NONE',  ( 79.99331838321626265, 55.99999999999999289, 4.966068647628683053 ) ) ;
#3294 = AXIS2_PLACEMENT_3D ( 'NONE', #16390, #748, #21507 ) ;
#3295 = AXIS2_PLACEMENT_3D ( 'NONE', #12700, #16615, #13152 ) ;
#3296 = CARTESIAN_POINT ( 'NONE',  ( 19.05734566456921542, 183.6057529188165915, 319.6991620761616559 ) ) ;
#3297 = EDGE_CURVE ( 'NONE', #16236, #13489, #8147, .T. ) ;
#3298 = DIRECTION ( 'NONE',  ( 0.4397038457472313144, 0.000000000000000000, -0.8981428216242086648 ) ) ;
#3299 = ORIENTED_EDGE ( 'NONE', *, *, #2591, .F. ) ;
#3300 = CARTESIAN_POINT ( 'NONE',  ( -88.40906079701869658, 78.43035437438882695, 33.14537955645111822 ) ) ;
#3301 = DIRECTION ( 'NONE',  ( 7.125109674159586684E-05, -0.9999848031710252272, 0.005512562950848869624 ) ) ;
#3302 = AXIS2_PLACEMENT_3D ( 'NONE', #8699, #12305, #9041 ) ;
#3303 = FACE_OUTER_BOUND ( 'NONE', #6567, .T. ) ;
#3304 = EDGE_CURVE ( 'NONE', #44, #19786, #15293, .T. ) ;
#3305 = AXIS2_PLACEMENT_3D ( 'NONE', #18113, #22072, #20025 ) ;
#3306 = CARTESIAN_POINT ( 'NONE',  ( 19.85645766388354971, -0.1201756712316815051, -11.23484659157417376 ) ) ;
#3308 = EDGE_LOOP ( 'NONE', ( #6133, #6546, #7347, #21466 ) ) ;
#3307 = ORIENTED_EDGE ( 'NONE', *, *, #8778, .T. ) ;
#3309 = CARTESIAN_POINT ( 'NONE',  ( 40.84145524218410372, 101.1708071963161615, 64.84331118128903881 ) ) ;
#3310 = CARTESIAN_POINT ( 'NONE',  ( 54.52327687265660927, 18.00000000000000355, 111.3697098814019029 ) ) ;
#3311 = CARTESIAN_POINT ( 'NONE',  ( 64.42223680557074772, 144.7550503794368524, -45.19787522242825162 ) ) ;
#3312 = DIRECTION ( 'NONE',  ( 0.000000000000000000, 0.000000000000000000, -1.000000000000000000 ) ) ;
#3313 = ORIENTED_EDGE ( 'NONE', *, *, #3503, .T. ) ;
#3314 = AXIS2_PLACEMENT_3D ( 'NONE', #4143, #718, #7713 ) ;
#3315 = EDGE_CURVE ( 'NONE', #13764, #19083, #1100, .T. ) ;
#3316 = ORIENTED_EDGE ( 'NONE', *, *, #19103, .T. ) ;
#3317 = DIRECTION ( 'NONE',  ( 0.01292394549866733230, 0.005513023399720419666, 0.9999012842304692006 ) ) ;
#3318 = CARTESIAN_POINT ( 'NONE',  ( -49.94445001183338917, 112.2316389946799120, -43.54034044231270428 ) ) ;
#3319 = VECTOR ( 'NONE', #11175, 1000.000000000000000 ) ;
#3320 = EDGE_LOOP ( 'NONE', ( #19313, #16483, #19262, #6872 ) ) ;
#3321 = EDGE_CURVE ( 'NONE', #858, #12094, #737, .T. ) ;
#3322 = CARTESIAN_POINT ( 'NONE',  ( 50.66019270109019601, 111.6821163282932190, -48.02485136456311210 ) ) ;
#3323 = ORIENTED_EDGE ( 'NONE', *, *, #17252, .F. ) ;
#3324 =( LENGTH_UNIT ( ) NAMED_UNIT ( * ) SI_UNIT ( .MILLI., .METRE. ) );
#3325 = AXIS2_PLACEMENT_3D ( 'NONE', #11563, #18784, #12008 ) ;
#3326 = CARTESIAN_POINT ( 'NONE',  ( -41.41899454747574083, 166.0889136240115249, 277.1829612759436827 ) ) ;
#3327 = DIRECTION ( 'NONE',  ( -7.125109674161246868E-05, 0.9999848031710252272, -0.005512562950850154186 ) ) ;
#3328 = CARTESIAN_POINT ( 'NONE',  ( 35.95309506732430549, 93.50464841319750064, 82.03286182426640494 ) ) ;
#3329 = ADVANCED_FACE ( 'NONE', ( #15053 ), #10302, .F. ) ;
#3330 = ORIENTED_EDGE ( 'NONE', *, *, #21023, .F. ) ;
#3331 = CARTESIAN_POINT ( 'NONE',  ( -40.54592687530145412, 169.7656965055118974, -41.97883890360929371 ) ) ;
#3332 =( NAMED_UNIT ( * ) SI_UNIT ( $, .STERADIAN. ) SOLID_ANGLE_UNIT ( ) );
#3333 = AXIS2_PLACEMENT_3D ( 'NONE', #10042, #14691, #6583 ) ;
#3334 = LINE ( 'NONE', #22594, #15400 ) ;
#3335 = ORIENTED_EDGE ( 'NONE', *, *, #10260, .T. ) ;
#3336 = CARTESIAN_POINT ( 'NONE',  ( -5.027868580402196308, 326.7615858019005373, 320.2878431667282371 ) ) ;
#3337 = ADVANCED_BREP_SHAPE_REPRESENTATION ( '', ( #9502, #6292 ), #9963 ) ;
#3338 = ORIENTED_EDGE ( 'NONE', *, *, #3273, .T. ) ;
#3339 = B_SPLINE_CURVE_WITH_KNOTS ( 'NONE', 3,
 ( #18520, #2782, #10463, #10352, #7124, #1963 ),
 .UNSPECIFIED., .F., .F.,
 ( 4, 2, 4 ),
 ( 0.000000000000000000, 0.0009977625019781909133, 0.001995525003956381827 ),
 .UNSPECIFIED. ) ;
#3340 = FACE_OUTER_BOUND ( 'NONE', #8742, .T. ) ;
#3341 = VECTOR ( 'NONE', #3945, 1000.000000000000227 ) ;
#3342 = CARTESIAN_POINT ( 'NONE',  ( -88.16361364164851011, 88.27739129944409058, 52.90104011961382469 ) ) ;
#3343 = EDGE_CURVE ( 'NONE', #4020, #17682, #17892, .T. ) ;
#3344 = AXIS2_PLACEMENT_3D ( 'NONE', #5265, #10456, #6878 ) ;
#3345 = FACE_OUTER_BOUND ( 'NONE', #13519, .T. ) ;
#3346 = VECTOR ( 'NONE', #13495, 999.9999999999998863 ) ;
#3347 = ORIENTED_EDGE ( 'NONE', *, *, #16474, .T. ) ;
#3348 = VERTEX_POINT ( 'NONE', #3085 ) ;
#3349 = DIRECTION ( 'NONE',  ( -0.000000000000000000, -1.000000000000000000, -0.000000000000000000 ) ) ;
#3350 = AXIS2_PLACEMENT_3D ( 'NONE', #10883, #17909, #7433 ) ;
#3351 = CARTESIAN_POINT ( 'NONE',  ( -36.07200259421443889, 94.02752048664967788, 83.44564859173975435 ) ) ;
#3352 = CARTESIAN_POINT ( 'NONE',  ( 41.99649215118846968, 170.0000000000000284, -0.5428139599949681759 ) ) ;
#3353 = ORIENTED_EDGE ( 'NONE', *, *, #20397, .T. ) ;
#3354 =( NAMED_UNIT ( * ) PLANE_ANGLE_UNIT ( ) SI_UNIT ( $, .RADIAN. ) );
#3355 = CARTESIAN_POINT ( 'NONE',  ( -19.99832959580404790, 170.0000000000008242, 0.2584828380936761705 ) ) ;
#3356 = FACE_OUTER_BOUND ( 'NONE', #17498, .T. ) ;
#3357 = VERTEX_POINT ( 'NONE', #10104 ) ;
#3358 = EDGE_CURVE ( 'NONE', #13022, #13585, #17113, .T. ) ;
#3359 = ORIENTED_EDGE ( 'NONE', *, *, #3708, .F. ) ;
#3360 = CARTESIAN_POINT ( 'NONE',  ( -12.65647975835393169, 184.5194971381093580, 278.5989247057070770 ) ) ;
#3361 = DIRECTION ( 'NONE',  ( 1.000000000000000000, 0.000000000000000000, 1.387778780781445676E-14 ) ) ;
#3362 = CARTESIAN_POINT ( 'NONE',  ( -58.84871535152515065, 114.6403824866543175, 163.0520739249805899 ) ) ;
#3363 = DIRECTION ( 'NONE',  ( 0.000000000000000000, 1.000000000000000000, -0.000000000000000000 ) ) ;
#3364 = CARTESIAN_POINT ( 'NONE',  ( 0.000000000000000000, 0.000000000000000000, 0.000000000000000000 ) ) ;
#3365 = AXIS2_PLACEMENT_3D ( 'NONE', #10262, #11545, #20708 ) ;
#3366 = VECTOR ( 'NONE', #5287, 1000.000000000000000 ) ;
#3367 = CARTESIAN_POINT ( 'NONE',  ( 105.0923722050658711, 70.19488773545521099, -32.49013605942705851 ) ) ;
#3368 = AXIS2_PLACEMENT_3D ( 'NONE', #5009, #8347, #22339 ) ;
#3369 = CARTESIAN_POINT ( 'NONE',  ( -63.99768274785666478, 99.80253851968858214, 77.96744723695394441 ) ) ;
#3370 = ORIENTED_EDGE ( 'NONE', *, *, #17786, .F. ) ;
#3371 = ORIENTED_EDGE ( 'NONE', *, *, #2623, .T. ) ;
#3372 = ORIENTED_EDGE ( 'NONE', *, *, #16567, .F. ) ;
#3373 = LINE ( 'NONE', #10159, #10433 ) ;
#3374 = ADVANCED_FACE ( 'NONE', ( #19494 ), #22460, .F. ) ;
#3375 = ADVANCED_FACE ( 'NONE', ( #5128 ), #19379, .F. ) ;
#3376 = VECTOR ( 'NONE', #5037, 1000.000000000000000 ) ;
#3377 = VERTEX_POINT ( 'NONE', #20758 ) ;
#3378 = VECTOR ( 'NONE', #6174, 1000.000000000000000 ) ;
#3379 = DIRECTION ( 'NONE',  ( 0.9999164797902017066, 6.965998958219365988E-18, -0.01292414190464157356 ) ) ;
#3380 = CARTESIAN_POINT ( 'NONE',  ( -90.03465221005033925, 70.01281497139055432, 63.19621350536183968 ) ) ;
#3381 = DIRECTION ( 'NONE',  ( -0.01292394549866632963, -0.005513023399716958026, -0.9999012842304692006 ) ) ;
#3382 = CARTESIAN_POINT ( 'NONE',  ( 40.93051939605364709, 108.3240682923980245, 71.73403676058168799 ) ) ;
#3383 = AXIS2_PLACEMENT_3D ( 'NONE', #19415, #9312, #11040 ) ;
#3384 = CARTESIAN_POINT ( 'NONE',  ( 86.24279638190517971, 74.99999999999998579, -1.114707239275309014 ) ) ;
#3385 = CARTESIAN_POINT ( 'NONE',  ( 12.83141560359293898, 190.4910289390495279, 307.8493993209711448 ) ) ;
#3386 = DIRECTION ( 'NONE',  ( -0.8608023089638389136, 0.002744228680570687078, 0.5089320721780778989 ) ) ;
#3387 = DIRECTION ( 'NONE',  ( 0.01292414190464131335, 1.902755938799530239E-22, 0.9999164797902015955 ) ) ;
#3388 = B_SPLINE_CURVE_WITH_KNOTS ( 'NONE', 3,
 ( #8565, #6842, #20849, #5106, #19765, #7506, #12790, #2210, #14423, #7849, #851, #503, #9336, #2559, #21386, #14879 ),
 .UNSPECIFIED., .F., .F.,
 ( 4, 2, 2, 2, 2, 2, 2, 4 ),
 ( 0.000000000000000000, 0.0003989366781685712302, 0.0007978733563371424604, 0.001196810034505713582, 0.001595746712674284921, 0.001994683390842856476, 0.002393620069011427164, 0.003191493425348539484 ),
 .UNSPECIFIED. ) ;
#3389 = APPLICATION_CONTEXT ( 'automotive_design' ) ;
#3390 = CARTESIAN_POINT ( 'NONE',  ( 90.41742102548467130, 80.31838830481380853, -32.51148913194525392 ) ) ;
#3391 = ORIENTED_EDGE ( 'NONE', *, *, #20902, .T. ) ;
#3392 =( NAMED_UNIT ( * ) PLANE_ANGLE_UNIT ( ) SI_UNIT ( $, .RADIAN. ) );
#3393 = AXIS2_PLACEMENT_3D ( 'NONE', #7168, #47, #11036 ) ;
#3394 = CONICAL_SURFACE ( 'NONE', #7063, 9.000000000000001776, 1.047197551196594301 ) ;
#3395 = CARTESIAN_POINT ( 'NONE',  ( 49.38251519867302619, 111.9218655255082382, -48.09675133120408219 ) ) ;
#3396 = CARTESIAN_POINT ( 'NONE',  ( -8.819172402740010241, 185.2124387659711999, 305.1895671936096619 ) ) ;
#3397 = VERTEX_POINT ( 'NONE', #15856 ) ;
#3398 = CARTESIAN_POINT ( 'NONE',  ( -91.28977804672278751, 78.08428866167092508, -30.31923231637458471 ) ) ;
#3399 = VERTEX_POINT ( 'NONE', #17691 ) ;
#3400 = EDGE_CURVE ( 'NONE', #2643, #17518, #20865, .T. ) ;
#3401 = VECTOR ( 'NONE', #12889, 1000.000000000000114 ) ;
#3402 = CARTESIAN_POINT ( 'NONE',  ( -14.02864438394168722, 325.7329298795136197, 320.4531201330285626 ) ) ;
#3403 =( BOUNDED_CURVE ( )  B_SPLINE_CURVE ( 3, ( #10190, #3069, #20636, #4891 ),
 .UNSPECIFIED., .F., .T. ) 
 B_SPLINE_CURVE_WITH_KNOTS ( ( 4, 4 ),
 ( 4.712388980384689674, 6.283185307179586232 ),
 .UNSPECIFIED. ) 
 CURVE ( )  GEOMETRIC_REPRESENTATION_ITEM ( )  RATIONAL_B_SPLINE_CURVE ( ( 1.000000000000000000, 0.8047378541243649375, 0.8047378541243649375, 1.000000000000000000 ) ) 
 REPRESENTATION_ITEM ( '' )  );
#3404 = CIRCLE ( 'NONE', #6707, 2.000000000000005329 ) ;
#3405 = AXIS2_PLACEMENT_3D ( 'NONE', #1360, #15380, #22328 ) ;
#3406 = CARTESIAN_POINT ( 'NONE',  ( 3.316624388958365088, 166.4147108432491109, 256.6009726804241495 ) ) ;
#3407 = CARTESIAN_POINT ( 'NONE',  ( 15.74005880004537872, 145.5104308052777640, 277.3467734109414664 ) ) ;
#3408 = VERTEX_POINT ( 'NONE', #13883 ) ;
#3409 = DIRECTION ( 'NONE',  ( 5.440186201345785633E-18, 1.000000000000000000, 1.334940939666367878E-17 ) ) ;
#3410 = ORIENTED_EDGE ( 'NONE', *, *, #17952, .F. ) ;
#3411 = ORIENTED_EDGE ( 'NONE', *, *, #13888, .T. ) ;
#3412 = CARTESIAN_POINT ( 'NONE',  ( -89.66113247980429435, 100.6041916471018709, -63.72504470331098503 ) ) ;
#3413 = PRODUCT_RELATED_PRODUCT_CATEGORY ( 'part', '', ( #5858 ) ) ;
#3414 = DIRECTION ( 'NONE',  ( 0.9999164797902015955, 2.001050586450178695E-22, -0.01292414190464131335 ) ) ;
#3415 = ORIENTED_EDGE ( 'NONE', *, *, #12655, .F. ) ;
#3416 = DIRECTION ( 'NONE',  ( 0.009760756503427813965, -0.9999378516499565217, 0.005387065077607405654 ) ) ;
#3417 = CARTESIAN_POINT ( 'NONE',  ( 85.01653497985981289, 104.3814432989690602, -69.80106575130697877 ) ) ;
#3418 = ORIENTED_EDGE ( 'NONE', *, *, #3070, .F. ) ;
#3419 = CARTESIAN_POINT ( 'NONE',  ( -72.51438462527775641, 87.23323244114081376, 69.92599951943640235 ) ) ;
#3420 = DIRECTION ( 'NONE',  ( -0.9999164797902017066, 1.387778780781447253E-14, 0.01292414190463832269 ) ) ;
#3421 = FACE_OUTER_BOUND ( 'NONE', #11045, .T. ) ;
#3422 = DIRECTION ( 'NONE',  ( 0.000000000000000000, 0.7071067811865456854, 0.7071067811865493491 ) ) ;
#3423 = AXIS2_PLACEMENT_3D ( 'NONE', #20142, #7977, #4414 ) ;
#3424 = VECTOR ( 'NONE', #11440, 1000.000000000000000 ) ;
#3425 = CARTESIAN_POINT ( 'NONE',  ( 20.69883497493187718, 181.8866873879648267, 314.4189726352637990 ) ) ;
#3426 = CARTESIAN_POINT ( 'NONE',  ( 13.77152037162459308, 159.1779343868491026, 324.5134547254186828 ) ) ;
#3427 = LINE ( 'NONE', #12291, #3440 ) ;
#3428 = ORIENTED_EDGE ( 'NONE', *, *, #6225, .T. ) ;
#3429 = EDGE_CURVE ( 'NONE', #21699, #10079, #3534, .T. ) ;
#3430 = DIRECTION ( 'NONE',  ( -5.440186201345738641E-18, -1.000000000000000000, -1.334940939666364181E-17 ) ) ;
#3431 = LINE ( 'NONE', #10328, #17717 ) ;
#3432 = DIRECTION ( 'NONE',  ( 1.000000000000000000, 0.000000000000000000, -9.912705577010318154E-17 ) ) ;
#3433 = AXIS2_PLACEMENT_3D ( 'NONE', #9583, #745, #13153 ) ;
#3434 = FACE_OUTER_BOUND ( 'NONE', #12563, .T. ) ;
#3435 = CARTESIAN_POINT ( 'NONE',  ( 11.51968368760321937, 174.5313030472551645, 323.7907258472187664 ) ) ;
#3436 = FACE_OUTER_BOUND ( 'NONE', #18085, .T. ) ;
#3437 = DIRECTION ( 'NONE',  ( 0.009760756503428003050, -0.9999378516499565217, 0.005387065077610373766 ) ) ;
#3438 = VERTEX_POINT ( 'NONE', #14359 ) ;
#3439 = DIRECTION ( 'NONE',  ( -3.987059982602682030E-17, -0.9455185755993167351, -0.3255681544571568109 ) ) ;
#3440 = VECTOR ( 'NONE', #22463, 1000.000000000000000 ) ;
#3441 = CARTESIAN_POINT ( 'NONE',  ( -50.37155587173380411, 112.6465223951286276, -43.53710749220883969 ) ) ;
#3442 = EDGE_CURVE ( 'NONE', #17368, #4929, #12632, .T. ) ;
#3443 = EDGE_LOOP ( 'NONE', ( #6648, #12270, #7216, #8861 ) ) ;
#3444 = CARTESIAN_POINT ( 'NONE',  ( 50.07407138682150816, 111.0341656543122184, -47.77903772492574319 ) ) ;
#3445 = EDGE_LOOP ( 'NONE', ( #21361, #7679, #1908, #5336 ) ) ;
#3446 = CARTESIAN_POINT ( 'NONE',  ( 106.7989984338461653, 79.11557862755608994, 26.34385626240403511 ) ) ;
#3447 = PLANE ( 'NONE',  #5038 ) ;
#3448 = DIRECTION ( 'NONE',  ( 0.009760756503427210282, -0.9999378516499566327, 0.005387065077606872227 ) ) ;
#3449 = EDGE_CURVE ( 'NONE', #9196, #2793, #6061, .T. ) ;
#3450 = PLANE ( 'NONE',  #2316 ) ;
#3451 = DIRECTION ( 'NONE',  ( -0.4397038457472424167, 0.000000000000000000, -0.8981428216242032248 ) ) ;
#3452 = CIRCLE ( 'NONE', #528, 2.499999999999988010 ) ;
#3453 = EDGE_LOOP ( 'NONE', ( #22641, #8728, #19679, #6787 ) ) ;
#3454 = CARTESIAN_POINT ( 'NONE',  ( 19.42790726798621748, 168.5114881856995623, 319.6178889223443775 ) ) ;
#3455 = VERTEX_POINT ( 'NONE', #14698 ) ;
#3456 = CIRCLE ( 'NONE', #5279, 3.099999999999998757 ) ;
#3457 = ADVANCED_FACE ( 'NONE', ( #9500 ), #5941, .T. ) ;
#3458 = VECTOR ( 'NONE', #5783, 1000.000000000000000 ) ;
#3459 = CARTESIAN_POINT ( 'NONE',  ( 44.00388087554392769, 168.0766615966952884, -77.35866297318138152 ) ) ;
#3460 = CARTESIAN_POINT ( 'NONE',  ( -88.16819192123389826, 88.65820917459086559, 52.48530130829333729 ) ) ;
#3461 = EDGE_CURVE ( 'NONE', #15089, #19786, #21253, .T. ) ;
#3462 = CARTESIAN_POINT ( 'NONE',  ( 5.178260401672350355, 158.1956848156823128, 324.6299402127509666 ) ) ;
#3463 = ORIENTED_EDGE ( 'NONE', *, *, #3461, .F. ) ;
#3464 = VERTEX_POINT ( 'NONE', #18028 ) ;
#3465 = DIRECTION ( 'NONE',  ( 7.125109674160258889E-05, -0.9999848031710252272, 0.005512562950849897447 ) ) ;
#3466 = CYLINDRICAL_SURFACE ( 'NONE', #18780, 2.000000000000001332 ) ;
#3467 = AXIS2_PLACEMENT_3D ( 'NONE', #22122, #6523, #15614 ) ;
#3468 = DIRECTION ( 'NONE',  ( -0.01292394549866745720, -0.005513023399720816918, -0.9999012842304692006 ) ) ;
#3469 = CARTESIAN_POINT ( 'NONE',  ( -41.41899454747574083, 166.0889136240115249, 277.1829612759436827 ) ) ;
#3470 = CARTESIAN_POINT ( 'NONE',  ( 84.44445234771735898, 75.03417954463949968, 1.461155955555357044 ) ) ;
#3471 = CYLINDRICAL_SURFACE ( 'NONE', #2715, 2.499999999999988010 ) ;
#3472 = ADVANCED_FACE ( 'NONE', ( #16083 ), #4096, .T. ) ;
#3473 = ORIENTED_EDGE ( 'NONE', *, *, #4996, .T. ) ;
#3474 = ORIENTED_EDGE ( 'NONE', *, *, #19142, .F. ) ;
#3475 = FACE_OUTER_BOUND ( 'NONE', #13358, .T. ) ;
#3476 = DIRECTION ( 'NONE',  ( 0.9999164797902017066, 2.001050586450178931E-22, -0.01292414190464131508 ) ) ;
#3477 = CARTESIAN_POINT ( 'NONE',  ( -12.99577148999190612, 164.7709424335249366, 311.5407534607413709 ) ) ;
#3478 = AXIS2_PLACEMENT_3D ( 'NONE', #22465, #18496, #15402 ) ;
#3479 = CARTESIAN_POINT ( 'NONE',  ( -106.0833544754548114, 79.13355406794943292, 29.09322962842180615 ) ) ;
#3480 = EDGE_CURVE ( 'NONE', #5690, #12459, #4380, .T. ) ;
#3481 = VERTEX_POINT ( 'NONE', #668 ) ;
#3482 = CARTESIAN_POINT ( 'NONE',  ( -110.8786557059970477, 104.3814432989690602, -67.26907703621752432 ) ) ;
#3483 = CARTESIAN_POINT ( 'NONE',  ( 3.575103298931712636, 166.5249713112435188, 276.5989983650335375 ) ) ;
#3484 = DIRECTION ( 'NONE',  ( 7.125109674364534776E-05, -0.9999848031710252272, 0.005512562950849704893 ) ) ;
#3485 = EDGE_LOOP ( 'NONE', ( #7503, #21513, #17440, #14077 ) ) ;
#3486 = AXIS2_PLACEMENT_3D ( 'NONE', #1181, #16592, #20220 ) ;
#3487 = ORIENTED_EDGE ( 'NONE', *, *, #10058, .F. ) ;
#3488 = EDGE_LOOP ( 'NONE', ( #22441, #19131, #11485, #11826 ) ) ;
#3489 = UNCERTAINTY_MEASURE_WITH_UNIT (LENGTH_MEASURE( 1.000000000000000082E-05 ), #4259, 'distance_accuracy_value', 'NONE');
#3490 = CARTESIAN_POINT ( 'NONE',  ( 18.76377268095312090, 185.1009473783541068, 310.9749437967080326 ) ) ;
#3491 = EDGE_CURVE ( 'NONE', #20616, #13170, #7315, .T. ) ;
#3492 = ORIENTED_EDGE ( 'NONE', *, *, #10051, .F. ) ;
#3493 = DIRECTION ( 'NONE',  ( 0.9999164797902015955, 6.965998958219364448E-18, -0.01292414190464157182 ) ) ;
#3494 = DIRECTION ( 'NONE',  ( 0.01292414190464131508, 0.000000000000000000, 0.9999164797902017066 ) ) ;
#3495 = CARTESIAN_POINT ( 'NONE',  ( -154.0000000000000000, 0.000000000000000000, 53.76161406891259986 ) ) ;
#3496 = CARTESIAN_POINT ( 'NONE',  ( 1.469576158976823671E-14, 23.00000000000000000, 120.0000000000000000 ) ) ;
#3497 = FILL_AREA_STYLE_COLOUR ( '', #13944 ) ;
#3498 = CIRCLE ( 'NONE', #8987, 112.5000000000000284 ) ;
#3499 = DIRECTION ( 'NONE',  ( 7.125109674364534776E-05, -0.9999848031710252272, 0.005512562950849704893 ) ) ;
#3500 = CARTESIAN_POINT ( 'NONE',  ( 12.88272372176025016, 190.4631953211766131, 307.8527186633484121 ) ) ;
#3501 = CARTESIAN_POINT ( 'NONE',  ( 91.23438425464441082, 78.34087653192547407, 30.69541483481418709 ) ) ;
#3502 = CARTESIAN_POINT ( 'NONE',  ( 91.86780221137911440, 79.10677575599459033, 26.44518439498796880 ) ) ;
#3503 = EDGE_CURVE ( 'NONE', #14111, #22024, #10997, .T. ) ;
#3504 = ORIENTED_EDGE ( 'NONE', *, *, #4006, .T. ) ;
#3505 = DIRECTION ( 'NONE',  ( -0.01246513159389404414, -0.2641402835564772844, -0.9644037178988117409 ) ) ;
#3506 = DIRECTION ( 'NONE',  ( 0.01292394549866733230, 0.005513023399720419666, 0.9999012842304692006 ) ) ;
#3507 = ORIENTED_EDGE ( 'NONE', *, *, #11084, .T. ) ;
#3508 = CARTESIAN_POINT ( 'NONE',  ( -90.50635355031123197, 79.35163122866377705, -27.25632624756008937 ) ) ;
#3509 = ORIENTED_EDGE ( 'NONE', *, *, #8994, .F. ) ;
#3510 = EDGE_CURVE ( 'NONE', #4020, #8155, #13945, .T. ) ;
#3511 = B_SPLINE_CURVE_WITH_KNOTS ( 'NONE', 3,
 ( #13331, #7674, #2747, #4330, #13435, #802, #4453, #9517 ),
 .UNSPECIFIED., .F., .F.,
 ( 4, 2, 2, 4 ),
 ( 0.002921157996826920233, 0.003648658589483134984, 0.004376159182139349735, 0.005831160367451864238 ),
 .UNSPECIFIED. ) ;
#3512 = AXIS2_PLACEMENT_3D ( 'NONE', #252, #14273, #4949 ) ;
#3513 = PRODUCT_DEFINITION_SHAPE ( 'NONE', 'NONE',  #22678 ) ;
#3514 = DIRECTION ( 'NONE',  ( 7.125109674160325297E-05, -0.9999848031710253382, 0.005512562950849327591 ) ) ;
#3515 = CARTESIAN_POINT ( 'NONE',  ( -56.88982296092829927, 126.2575686056374735, 47.57983110662551951 ) ) ;
#3516 = DIRECTION ( 'NONE',  ( -0.3101392564284290998, -0.9506461370142487155, 0.009250070373107117244 ) ) ;
#3517 = DIRECTION ( 'NONE',  ( -0.9934404589540163366, -0.1135548637187055454, 0.01346653032743023483 ) ) ;
#3518 = ORIENTED_EDGE ( 'NONE', *, *, #6996, .F. ) ;
#3519 = PLANE ( 'NONE',  #348 ) ;
#3520 = ORIENTED_EDGE ( 'NONE', *, *, #11394, .F. ) ;
#3521 = CARTESIAN_POINT ( 'NONE',  ( -14.93612093091044102, 185.1121758471145142, 276.7357782268812798 ) ) ;
#3522 = DIRECTION ( 'NONE',  ( 0.01292394549866738955, 0.005513023399720468239, 0.9999012842304693116 ) ) ;
#3523 = CARTESIAN_POINT ( 'NONE',  ( 70.91392079944854743, 91.17157287525388654, 84.09052168258639881 ) ) ;
#3524 = ADVANCED_FACE ( 'NONE', ( #13091, #7440, #9150 ), #3877, .T. ) ;
#3525 = CARTESIAN_POINT ( 'NONE',  ( -10.61849163981879762, 184.1265005819461464, 321.1111245915606105 ) ) ;
#3526 = EDGE_CURVE ( 'NONE', #5966, #15010, #21445, .T. ) ;
#3527 = DIRECTION ( 'NONE',  ( 0.01292394549866728373, 0.005513023399720296501, 0.9999012842304693116 ) ) ;
#3528 = CARTESIAN_POINT ( 'NONE',  ( -12.58378492319879527, 109.7167104967248434, 130.3428598364639299 ) ) ;
#3529 = VERTEX_POINT ( 'NONE', #21652 ) ;
#3530 = DIRECTION ( 'NONE',  ( -5.440186201345738641E-18, -1.000000000000000000, -1.334940939666364181E-17 ) ) ;
#3531 = PLANE ( 'NONE',  #9914 ) ;
#3532 = DIRECTION ( 'NONE',  ( 0.01035335185279138807, 0.005513005182356417802, 0.9999312050732649393 ) ) ;
#3533 = LINE ( 'NONE', #17008, #13609 ) ;
#3534 = LINE ( 'NONE', #10546, #3279 ) ;
#3535 = FACE_OUTER_BOUND ( 'NONE', #15370, .T. ) ;
#3536 = DIRECTION ( 'NONE',  ( 7.125109674364534776E-05, -0.9999848031710252272, 0.005512562950849704893 ) ) ;
#3537 = CARTESIAN_POINT ( 'NONE',  ( 87.98413419613014241, 100.6041916471018851, -66.02114910964037620 ) ) ;
#3538 = DIRECTION ( 'NONE',  ( 7.125109674161246868E-05, -0.9999848031710253382, 0.005512562950850155054 ) ) ;
#3539 = CARTESIAN_POINT ( 'NONE',  ( -66.42308629463825298, 169.3906321239456361, -109.6814500331617381 ) ) ;
#3540 = CARTESIAN_POINT ( 'NONE',  ( -50.60480870902609496, 108.7763774210405501, -45.65653423414172352 ) ) ;
#3541 = LINE ( 'NONE', #10555, #7251 ) ;
#3542 = DIRECTION ( 'NONE',  ( 0.01292394549866733230, 0.005513023399720419666, 0.9999012842304692006 ) ) ;
#3543 = DIRECTION ( 'NONE',  ( 7.125109674160258889E-05, -0.9999848031710252272, 0.005512562950849897447 ) ) ;
#3544 = CIRCLE ( 'NONE', #6124, 1.999999999999997335 ) ;
#3545 = EDGE_LOOP ( 'NONE', ( #21188, #6956, #16754, #21492 ) ) ;
#3546 = CARTESIAN_POINT ( 'NONE',  ( 157.5176307659771169, 20.00000000000000000, 60.94675664190834397 ) ) ;
#3547 = DIRECTION ( 'NONE',  ( 0.000000000000000000, 1.000000000000000000, -0.000000000000000000 ) ) ;
#3548 = CARTESIAN_POINT ( 'NONE',  ( 58.09936094630035797, 143.2573102595451928, 45.99984121742717491 ) ) ;
#3549 = ADVANCED_FACE ( 'NONE', ( #12736 ), #4317, .F. ) ;
#3550 = EDGE_LOOP ( 'NONE', ( #12061, #4150, #15674, #19616 ) ) ;
#3551 = CARTESIAN_POINT ( 'NONE',  ( 50.28732129150708374, 111.3287588133958081, -47.88997685343035471 ) ) ;
#3552 = ORIENTED_EDGE ( 'NONE', *, *, #3872, .T. ) ;
#3553 = CARTESIAN_POINT ( 'NONE',  ( -9.381793152695545146, 70.09252763182296064, -94.06097113112909369 ) ) ;
#3554 = DIRECTION ( 'NONE',  ( 0.01292394549866731669, 0.005513023399720593139, 0.9999012842304692006 ) ) ;
#3555 = DIRECTION ( 'NONE',  ( -0.01292414190463992904, -1.902755938799528123E-22, -0.9999164797902017066 ) ) ;
#3556 = DIRECTION ( 'NONE',  ( 7.125109674364534776E-05, -0.9999848031710252272, 0.005512562950849704893 ) ) ;
#3557 = SURFACE_STYLE_FILL_AREA ( #19293 ) ;
#3558 = ORIENTED_EDGE ( 'NONE', *, *, #12537, .F. ) ;
#3559 = VECTOR ( 'NONE', #3132, 999.9999999999998863 ) ;
#3560 = CARTESIAN_POINT ( 'NONE',  ( 18.14299768316436001, 168.3676586590315765, 320.3890303468865000 ) ) ;
#3561 = CARTESIAN_POINT ( 'NONE',  ( 17.53646115355174828, 187.5322632972278711, 275.9756305834653176 ) ) ;
#3562 = ORIENTED_EDGE ( 'NONE', *, *, #1372, .F. ) ;
#3563 = CARTESIAN_POINT ( 'NONE',  ( -10.95382118728218224, 81.44091995301859299, -92.00507013140021684 ) ) ;
#3564 = EDGE_CURVE ( 'NONE', #9861, #17867, #21980, .T. ) ;
#3565 = CARTESIAN_POINT ( 'NONE',  ( -89.73902452844515665, 89.01173883974765033, 52.00261209584472510 ) ) ;
#3567 = ORIENTED_EDGE ( 'NONE', *, *, #15857, .T. ) ;
#3566 = ORIENTED_EDGE ( 'NONE', *, *, #7415, .T. ) ;
#3568 = VERTEX_POINT ( 'NONE', #2500 ) ;
#3569 = CARTESIAN_POINT ( 'NONE',  ( 161.9999999999998579, 0.000000000000000000, 10.00000000000220091 ) ) ;
#3570 = CARTESIAN_POINT ( 'NONE',  ( -41.83656076456451700, 165.9107905944781862, 244.8766507330992681 ) ) ;
#3571 = PLANE ( 'NONE',  #3138 ) ;
#3572 = AXIS2_PLACEMENT_3D ( 'NONE', #20438, #17237, #4693 ) ;
#3573 = CARTESIAN_POINT ( 'NONE',  ( -104.8202145123291018, 69.99999999999998579, 33.35749735200943178 ) ) ;
#3574 = ORIENTED_EDGE ( 'NONE', *, *, #11205, .F. ) ;
#3575 = CARTESIAN_POINT ( 'NONE',  ( 20.38408663817444477, 184.0728056720850532, 276.2849873611855855 ) ) ;
#3576 = VERTEX_POINT ( 'NONE', #21541 ) ;
#3577 = LINE ( 'NONE', #2093, #20315 ) ;
#3578 = CARTESIAN_POINT ( 'NONE',  ( -77.82735487582385758, 75.11374352463818127, 5.654166264129496078 ) ) ;
#3579 = B_SPLINE_CURVE_WITH_KNOTS ( 'NONE', 3,
 ( #6238, #15331, #9805, #8397, #2692, #20461, #4618, #6574, #22181, #9698, #18862, #13593, #11536, #15443, #1076, #22060, #3012, #20576 ),
 .UNSPECIFIED., .F., .F.,
 ( 4, 2, 2, 2, 2, 2, 2, 2, 4 ),
 ( 0.000000000000000000, 0.0007972436847030672444, 0.001594487369406134489, 0.002391731054109201733, 0.003188974738812268978, 0.003986218423515336222, 0.004783462108218403466, 0.005580705792921470711, 0.006377949477624537955 ),
 .UNSPECIFIED. ) ;
#3580 = CARTESIAN_POINT ( 'NONE',  ( -24.57841208749768924, 324.5249605026011182, 320.0802301758413364 ) ) ;
#3581 = ADVANCED_FACE ( 'NONE', ( #560 ), #1408, .F. ) ;
#3582 = EDGE_LOOP ( 'NONE', ( #4918, #19219 ) ) ;
#3583 = EDGE_CURVE ( 'NONE', #7781, #17835, #10471, .T. ) ;
#3584 = LINE ( 'NONE', #10593, #14733 ) ;
#3585 = CARTESIAN_POINT ( 'NONE',  ( -38.69757710431294839, 94.02752048664900997, -82.47923521851862461 ) ) ;
#3586 = CARTESIAN_POINT ( 'NONE',  ( 89.23620587891578282, 78.43035437438882695, 30.84927515012174482 ) ) ;
#3587 = CARTESIAN_POINT ( 'NONE',  ( 105.2816027134186498, 70.66149885336976411, -31.87151722101071272 ) ) ;
#3588 = VERTEX_POINT ( 'NONE', #16655 ) ;
#3589 = PLANE ( 'NONE',  #6302 ) ;
#3590 = EDGE_LOOP ( 'NONE', ( #17791, #3335, #7224, #12989 ) ) ;
#3591 = ORIENTED_EDGE ( 'NONE', *, *, #20551, .F. ) ;
#3592 = ADVANCED_FACE ( 'NONE', ( #907 ), #11686, .F. ) ;
#3593 = CARTESIAN_POINT ( 'NONE',  ( 19.06930845108338701, 184.8361062471226717, 317.3053272177560871 ) ) ;
#3594 = EDGE_CURVE ( 'NONE', #10934, #4883, #2498, .T. ) ;
#3595 = ORIENTED_EDGE ( 'NONE', *, *, #13094, .T. ) ;
#3596 = EDGE_CURVE ( 'NONE', #7779, #21740, #21595, .T. ) ;
#3597 = DIRECTION ( 'NONE',  ( -0.9999164797902015955, -4.476705744456268255E-15, 0.01292414190464141917 ) ) ;
#3598 = FACE_OUTER_BOUND ( 'NONE', #8961, .T. ) ;
#3599 = CARTESIAN_POINT ( 'NONE',  ( -14.37471740060550118, 109.6998846769365628, 127.3137863664913425 ) ) ;
#3600 = VECTOR ( 'NONE', #15211, 1000.000000000000000 ) ;
#3601 = PLANE ( 'NONE',  #6733 ) ;
#3602 = CARTESIAN_POINT ( 'NONE',  ( -38.85108570016819129, 97.00796024230733394, 84.16132632256042712 ) ) ;
#3603 = CARTESIAN_POINT ( 'NONE',  ( 84.64642305175908632, 75.08946592368292272, -5.226459242126186844 ) ) ;
#3604 = CARTESIAN_POINT ( 'NONE',  ( 14.21959016068815274, 186.7523085471082709, 307.8325657923471681 ) ) ;
#3605 = CARTESIAN_POINT ( 'NONE',  ( 91.69412133380886587, 80.03889463955920291, 29.36066737363380241 ) ) ;
#3606 = ADVANCED_FACE ( 'NONE', ( #613 ), #2205, .T. ) ;
#3607 = VECTOR ( 'NONE', #16039, 1000.000000000000000 ) ;
#3608 = EDGE_CURVE ( 'NONE', #19550, #8739, #20586, .T. ) ;
#3609 = CARTESIAN_POINT ( 'NONE',  ( 89.99332827845005056, 79.52815953299851515, 27.82019389467122750 ) ) ;
#3610 = EDGE_CURVE ( 'NONE', #160, #3984, #6107, .T. ) ;
#3611 = LINE ( 'NONE', #3944, #10665 ) ;
#3612 = CARTESIAN_POINT ( 'NONE',  ( -1.163172771417702478, 87.00000000000001421, -89.99248318111824574 ) ) ;
#3613 = EDGE_LOOP ( 'NONE', ( #6256, #194, #9915, #11286 ) ) ;
#3614 = CARTESIAN_POINT ( 'NONE',  ( -92.94153934368371495, 77.13727434530990479, -28.81475843614325782 ) ) ;
#3615 = AXIS2_PLACEMENT_3D ( 'NONE', #3352, #6792, #1313 ) ;
#3616 = ORIENTED_EDGE ( 'NONE', *, *, #22300, .T. ) ;
#3617 = VECTOR ( 'NONE', #8185, 1000.000000000000114 ) ;
#3618 = EDGE_CURVE ( 'NONE', #10046, #16057, #11285, .T. ) ;
#3619 = CARTESIAN_POINT ( 'NONE',  ( -70.22615711568091967, 70.59893530615325119, -84.66585046671893622 ) ) ;
#3620 = EDGE_CURVE ( 'NONE', #10079, #10627, #21493, .T. ) ;
#3621 = FACE_OUTER_BOUND ( 'NONE', #7261, .T. ) ;
#3622 = FACE_BOUND ( 'NONE', #10317, .T. ) ;
#3623 = CARTESIAN_POINT ( 'NONE',  ( -14.53254043310009358, 177.6255169206013989, 113.6379760112694584 ) ) ;
#3624 = ORIENTED_EDGE ( 'NONE', *, *, #7185, .T. ) ;
#3625 = CARTESIAN_POINT ( 'NONE',  ( 1.364374644014609697E-14, 69.99999999999998579, -9.836443712999143722E-15 ) ) ;
#3626 = ORIENTED_EDGE ( 'NONE', *, *, #18645, .F. ) ;
#3627 = DIRECTION ( 'NONE',  ( -0.01292394549866731669, -0.005513023399720593139, -0.9999012842304692006 ) ) ;
#3628 = VECTOR ( 'NONE', #4347, 1000.000000000000114 ) ;
#3629 = EDGE_CURVE ( 'NONE', #12879, #6995, #2446, .T. ) ;
#3630 = CARTESIAN_POINT ( 'NONE',  ( -10.79665701538697320, 105.7314194667820004, 132.9990107322359449 ) ) ;
#3631 = CARTESIAN_POINT ( 'NONE',  ( -12.01575389182707632, 182.4076787623489793, 322.7174846376827873 ) ) ;
#3632 = VECTOR ( 'NONE', #20078, 1000.000000000000000 ) ;
#3634 = LINE ( 'NONE', #10647, #14284 ) ;
#3633 = CARTESIAN_POINT ( 'NONE',  ( -13.36217923100928928, 326.0172268059896510, 372.0162718331554288 ) ) ;
#3635 = CARTESIAN_POINT ( 'NONE',  ( -11.14759061400257423, 137.5759562808229362, 104.7141423461399086 ) ) ;
#3636 = ORIENTED_EDGE ( 'NONE', *, *, #20441, .F. ) ;
#3637 = CARTESIAN_POINT ( 'NONE',  ( -12.26418779587024588, 185.2816307007135492, 308.8815972836887340 ) ) ;
#3638 = DIRECTION ( 'NONE',  ( -0.01292414190464131508, -1.902755938799530474E-22, -0.9999164797902017066 ) ) ;
#3639 = FACE_OUTER_BOUND ( 'NONE', #14179, .T. ) ;
#3640 = CARTESIAN_POINT ( 'NONE',  ( -12.58827034560151681, 181.8529111828999589, 320.1441755304902586 ) ) ;
#3641 = CARTESIAN_POINT ( 'NONE',  ( 12.36154785051915894, 187.5489770926929793, 304.9204778021706375 ) ) ;
#3642 = LINE ( 'NONE', #5016, #12660 ) ;
#3643 = ORIENTED_EDGE ( 'NONE', *, *, #6245, .F. ) ;
#3644 = AXIS2_PLACEMENT_3D ( 'NONE', #7146, #15360, #20610 ) ;
#3645 = CIRCLE ( 'NONE', #19420, 5.000000000000023981 ) ;
#3646 = CYLINDRICAL_SURFACE ( 'NONE', #18442, 3.399999999999992806 ) ;
#3647 = ADVANCED_FACE ( 'NONE', ( #9435 ), #22631, .T. ) ;
#3648 = ADVANCED_FACE ( 'NONE', ( #9684 ), #17559, .T. ) ;
#3649 = DIRECTION ( 'NONE',  ( -0.01292414190464131335, -1.902755938799530239E-22, -0.9999164797902015955 ) ) ;
#3650 = AXIS2_PLACEMENT_3D ( 'NONE', #17809, #10436, #17913 ) ;
#3651 = ORIENTED_EDGE ( 'NONE', *, *, #18976, .F. ) ;
#3652 = DIRECTION ( 'NONE',  ( 0.000000000000000000, 0.000000000000000000, 1.000000000000000000 ) ) ;
#3653 = DIRECTION ( 'NONE',  ( 0.8981428216242027807, 0.000000000000000000, -0.4397038457472431938 ) ) ;
#3654 = DIRECTION ( 'NONE',  ( -5.440186201345738641E-18, -1.000000000000000000, -1.334940939666364181E-17 ) ) ;
#3655 = CARTESIAN_POINT ( 'NONE',  ( 53.22065341430143803, 129.3749911766419700, 248.8527623646411939 ) ) ;
#3656 = ORIENTED_EDGE ( 'NONE', *, *, #9205, .F. ) ;
#3657 = CARTESIAN_POINT ( 'NONE',  ( -50.99271059757531788, 113.0670368246753554, -43.53139746460606574 ) ) ;
#3658 = ORIENTED_EDGE ( 'NONE', *, *, #14168, .T. ) ;
#3659 = VERTEX_POINT ( 'NONE', #5756 ) ;
#3660 = CARTESIAN_POINT ( 'NONE',  ( -8.312614011469616315, 69.99999999999998579, -95.45924547291811280 ) ) ;
#3661 = CARTESIAN_POINT ( 'NONE',  ( -55.33804461215960657, 114.2193244133317904, 167.6379947637574617 ) ) ;
#3662 = CARTESIAN_POINT ( 'NONE',  ( -5.731715098087014404, 326.6288426432528240, 307.3396573775339107 ) ) ;
#3663 = VECTOR ( 'NONE', #3414, 1000.000000000000114 ) ;
#3664 = AXIS2_PLACEMENT_3D ( 'NONE', #6016, #16384, #16275 ) ;
#3665 = ORIENTED_EDGE ( 'NONE', *, *, #4286, .T. ) ;
#3666 = DIRECTION ( 'NONE',  ( 0.000000000000000000, 0.000000000000000000, 1.000000000000000000 ) ) ;
#3667 = LINE ( 'NONE', #582, #19624 ) ;
#3668 = AXIS2_PLACEMENT_3D ( 'NONE', #12876, #14732, #5972 ) ;
#3669 = CARTESIAN_POINT ( 'NONE',  ( -2.207300919685918128, 327.0790409159932892, 319.0232558455138587 ) ) ;
#3670 = EDGE_LOOP ( 'NONE', ( #16266, #5053, #5703, #9149 ) ) ;
#3671 = DIRECTION ( 'NONE',  ( 0.7968670734554454960, -0.4220031449644340849, -0.4323380770677970331 ) ) ;
#3672 = CARTESIAN_POINT ( 'NONE',  ( -90.02167563947240581, 87.67692088304698927, 50.98541494077212377 ) ) ;
#3673 = ORIENTED_EDGE ( 'NONE', *, *, #10099, .T. ) ;
#3674 = VECTOR ( 'NONE', #3422, 1000.000000000000000 ) ;
#3675 =( REPRESENTATION_RELATIONSHIP ('NONE','NONE', #11808, #21889 ) REPRESENTATION_RELATIONSHIP_WITH_TRANSFORMATION ( #15517 )SHAPE_REPRESENTATION_RELATIONSHIP( ) );
#3676 = VERTEX_POINT ( 'NONE', #6222 ) ;
#3677 = CARTESIAN_POINT ( 'NONE',  ( -41.88967587883006871, 162.6016759231961260, 277.2082720574355790 ) ) ;
#3678 = VECTOR ( 'NONE', #22146, 1000.000000000000000 ) ;
#3679 = CARTESIAN_POINT ( 'NONE',  ( 17.43893902918902938, 177.6144908738019694, 111.2246009018600006 ) ) ;
#3680 = AXIS2_PLACEMENT_3D ( 'NONE', #3364, #1654, #5692 ) ;
#3681 = CARTESIAN_POINT ( 'NONE',  ( 82.60421184180059129, 75.10273324658503213, 3.350270875632189505 ) ) ;
#3682 = CARTESIAN_POINT ( 'NONE',  ( -1.386679829960242619E-13, 2.000000000000000000, -9.999999999999994671 ) ) ;
#3683 = ORIENTED_EDGE ( 'NONE', *, *, #16815, .F. ) ;
#3684 = CARTESIAN_POINT ( 'NONE',  ( 79.99331838321626265, 102.0000000000000000, 3.966068647628679500 ) ) ;
#3685 = CONICAL_SURFACE ( 'NONE', #8448, 24.99999999999998224, 0.03490658503988662564 ) ;
#3686 = ORIENTED_EDGE ( 'NONE', *, *, #2069, .T. ) ;
#3687 = DIRECTION ( 'NONE',  ( -0.9999164797902015955, -4.653667080246434899E-16, 0.01292414190464084844 ) ) ;
#3688 = DIRECTION ( 'NONE',  ( 0.9999164797902015955, 6.965998958219364448E-18, -0.01292414190464157182 ) ) ;
#3689 = CARTESIAN_POINT ( 'NONE',  ( 3.086109933851330151E-14, 1.999999999999998224, 126.0000000000000000 ) ) ;
#3690 = CARTESIAN_POINT ( 'NONE',  ( -13.39934810366954210, 164.7282670150663080, 312.4024525391586735 ) ) ;
#3691 = ORIENTED_EDGE ( 'NONE', *, *, #1226, .F. ) ;
#3692 = CARTESIAN_POINT ( 'NONE',  ( -105.6047345086702336, 78.54962563481552706, 30.78394349069507996 ) ) ;
#3693 = ORIENTED_EDGE ( 'NONE', *, *, #2384, .T. ) ;
#3694 = CARTESIAN_POINT ( 'NONE',  ( 91.62437796271728985, 71.80839515725416788, 60.86849236629024062 ) ) ;
#3695 = AXIS2_PLACEMENT_3D ( 'NONE', #21587, #2326, #11054 ) ;
#3696 = CARTESIAN_POINT ( 'NONE',  ( -50.18853567905175339, 114.4097660515002985, 166.1373319179420207 ) ) ;
#3697 = ORIENTED_EDGE ( 'NONE', *, *, #21017, .F. ) ;
#3698 = PRODUCT_DEFINITION_SHAPE ( 'NONE', 'NONE',  #22699 ) ;
#3699 = VECTOR ( 'NONE', #875, 1000.000000000000000 ) ;
#3700 = AXIS2_PLACEMENT_3D ( 'NONE', #14520, #2194, #16127 ) ;
#3701 = LINE ( 'NONE', #10722, #17684 ) ;
#3702 = ORIENTED_EDGE ( 'NONE', *, *, #9562, .F. ) ;
#3703 = VERTEX_POINT ( 'NONE', #846 ) ;
#3704 = EDGE_LOOP ( 'NONE', ( #8453, #9703 ) ) ;
#3705 = UNCERTAINTY_MEASURE_WITH_UNIT (LENGTH_MEASURE( 1.000000000000000082E-05 ), #14811, 'distance_accuracy_value', 'NONE');
#3706 = CARTESIAN_POINT ( 'NONE',  ( 19.42556530730579567, 136.7551719540686008, -44.57217540897067920 ) ) ;
#3707 = AXIS2_PLACEMENT_3D ( 'NONE', #12500, #10648, #16312 ) ;
#3708 = EDGE_CURVE ( 'NONE', #4043, #8178, #9457, .T. ) ;
#3709 = ORIENTED_EDGE ( 'NONE', *, *, #13878, .F. ) ;
#3710 = PLANE ( 'NONE',  #9474 ) ;
#3711 = CARTESIAN_POINT ( 'NONE',  ( -88.74294073166163344, 70.70905333810220839, 62.85632276041776123 ) ) ;
#3712 = CARTESIAN_POINT ( 'NONE',  ( -12.73484320226976863, 148.6269210710419486, 278.8388817128882238 ) ) ;
#3713 = CARTESIAN_POINT ( 'NONE',  ( 395.1215762121263992, 103.0000000000000000, -76.28455149755049547 ) ) ;
#3714 = AXIS2_PLACEMENT_3D ( 'NONE', #7158, #7374, #14069 ) ;
#3715 = CARTESIAN_POINT ( 'NONE',  ( -41.67747345744867715, 165.9786531560170033, 257.1849355913340673 ) ) ;
#3716 = PRODUCT_DEFINITION_SHAPE ( 'NONE', 'NONE',  #2728 ) ;
#3717 = ORIENTED_EDGE ( 'NONE', *, *, #8400, .F. ) ;
#3718 = PRESENTATION_STYLE_ASSIGNMENT (( #7276 ) ) ;
#3719 = CARTESIAN_POINT ( 'NONE',  ( 76.62183188433269265, 75.14843384332513665, -6.300527722194164681 ) ) ;
#3720 = AXIS2_PLACEMENT_3D ( 'NONE', #12103, #3021, #13720 ) ;
#3721 = CARTESIAN_POINT ( 'NONE',  ( 15.52111512002419502, 188.5491499182944608, 308.4788755532068194 ) ) ;
#3722 = CARTESIAN_POINT ( 'NONE',  ( 92.67786813602299389, 77.16999450923081838, 28.87226322141187040 ) ) ;
#3723 = ADVANCED_FACE ( 'NONE', ( #5999 ), #20104, .T. ) ;
#3724 = DIRECTION ( 'NONE',  ( 0.01292394549866728200, 0.005513023399720295634, 0.9999012842304692006 ) ) ;
#3725 = CIRCLE ( 'NONE', #12165, 9.000000000000001776 ) ;
#3726 = ADVANCED_FACE ( 'NONE', ( #14530, #4489, #19763 ), #13039, .F. ) ;
#3727 = B_SPLINE_CURVE_WITH_KNOTS ( 'NONE', 3,
 ( #8680, #3082, #20866, #94 ),
 .UNSPECIFIED., .F., .F.,
 ( 4, 4 ),
 ( 0.0009630630797684288464, 0.007033511846324326695 ),
 .UNSPECIFIED. ) ;
#3728 = EDGE_CURVE ( 'NONE', #19631, #5033, #9561, .T. ) ;
#3729 = CARTESIAN_POINT ( 'NONE',  ( 48.58946335778052372, 189.4003865961453812, -109.4536762928195230 ) ) ;
#3730 = CARTESIAN_POINT ( 'NONE',  ( -41.52238611146465530, 166.0448094368136935, 269.1837510020998820 ) ) ;
#3731 = ORIENTED_EDGE ( 'NONE', *, *, #5044, .F. ) ;
#3733 = CARTESIAN_POINT ( 'NONE',  ( -89.40485731804325553, 79.89806915697583634, -28.95844815008361905 ) ) ;
#3732 = AXIS2_PLACEMENT_3D ( 'NONE', #8705, #12652, #21233 ) ;
#3734 = EDGE_LOOP ( 'NONE', ( #9958, #4107 ) ) ;
#3735 = ORIENTED_EDGE ( 'NONE', *, *, #13178, .T. ) ;
#3736 = AXIS2_PLACEMENT_3D ( 'NONE', #11014, #5614, #12859 ) ;
#3737 = AXIS2_PLACEMENT_3D ( 'NONE', #2536, #9665, #14739 ) ;
#3738 = ADVANCED_FACE ( 'NONE', ( #14876 ), #21817, .T. ) ;
#3739 = ADVANCED_FACE ( 'NONE', ( #22377 ), #6780, .T. ) ;
#3740 = DIRECTION ( 'NONE',  ( -0.01292414190464131335, -1.902755938799530239E-22, -0.9999164797902015955 ) ) ;
#3741 = EDGE_CURVE ( 'NONE', #13237, #5372, #296, .T. ) ;
#3743 = EDGE_CURVE ( 'NONE', #11172, #2955, #20824, .T. ) ;
#3742 = EDGE_LOOP ( 'NONE', ( #1800, #1220, #22064, #18020 ) ) ;
#3744 = CARTESIAN_POINT ( 'NONE',  ( 14.19595143612763444, 113.7230284608895943, 131.1317842058634255 ) ) ;
#3745 = DIRECTION ( 'NONE',  ( 0.009760756503427210282, -0.9999378516499566327, 0.005387065077606872227 ) ) ;
#3746 = ORIENTED_EDGE ( 'NONE', *, *, #21604, .T. ) ;
#3747 = PLANE ( 'NONE',  #18331 ) ;
#3748 = VERTEX_POINT ( 'NONE', #9791 ) ;
#3749 = ORIENTED_EDGE ( 'NONE', *, *, #8631, .T. ) ;
#3750 = VECTOR ( 'NONE', #11841, 999.9999999999998863 ) ;
#3751 = CARTESIAN_POINT ( 'NONE',  ( -16.82677409528017520, 137.4993252555668164, 90.88659727581192271 ) ) ;
#3752 = AXIS2_PLACEMENT_3D ( 'NONE', #8932, #12492, #7213 ) ;
#3753 = VECTOR ( 'NONE', #13380, 1000.000000000000227 ) ;
#3754 = EDGE_CURVE ( 'NONE', #19631, #4929, #17172, .T. ) ;
#3755 = DIRECTION ( 'NONE',  ( 0.007270543169446074330, 0.7109943187548881660, 0.7031601651830782229 ) ) ;
#3756 = CARTESIAN_POINT ( 'NONE',  ( -11.04227196300320912, 183.6076801826763187, 320.9867185712774926 ) ) ;
#3757 = CARTESIAN_POINT ( 'NONE',  ( -88.55041925572842842, 79.97987315375630146, 31.50236046386196165 ) ) ;
#3758 = DIRECTION ( 'NONE',  ( -7.125109674403282806E-05, 0.9999848031710253382, -0.005512562950848280685 ) ) ;
#3759 = EDGE_CURVE ( 'NONE', #21389, #17449, #679, .T. ) ;
#3760 = ORIENTED_EDGE ( 'NONE', *, *, #20023, .F. ) ;
#3761 = CARTESIAN_POINT ( 'NONE',  ( -61.06284936382945716, 114.6696180983937410, 168.3840612900001190 ) ) ;
#3762 = EDGE_CURVE ( 'NONE', #21685, #9499, #11859, .T. ) ;
#3763 = DIRECTION ( 'NONE',  ( 0.01292394549866733230, 0.005513023399720419666, 0.9999012842304692006 ) ) ;
#3764 = AXIS2_PLACEMENT_3D ( 'NONE', #8596, #13682, #22251 ) ;
#3765 = DIRECTION ( 'NONE',  ( 0.01292394549866740169, 0.005513023399720822990, 0.9999012842304693116 ) ) ;
#3766 = CARTESIAN_POINT ( 'NONE',  ( -15.18603124401100679, 179.4839357967852607, 314.7101063110252426 ) ) ;
#3767 = DIRECTION ( 'NONE',  ( -2.025474946048326393E-22, 1.000000000000000000, -1.876735158486679873E-22 ) ) ;
#3768 = VECTOR ( 'NONE', #14937, 1000.000000000000114 ) ;
#3769 = AXIS2_PLACEMENT_3D ( 'NONE', #6347, #13696, #11966 ) ;
#3770 = CARTESIAN_POINT ( 'NONE',  ( -38.77166272639713185, 129.3749911766419700, 250.0417834198682101 ) ) ;
#3771 = EDGE_CURVE ( 'NONE', #7184, #17163, #10943, .T. ) ;
#3772 = EDGE_LOOP ( 'NONE', ( #2103, #9863, #21778, #6767 ) ) ;
#3773 = DIRECTION ( 'NONE',  ( 5.440186201345785633E-18, 1.000000000000000000, 1.334940939666367878E-17 ) ) ;
#3774 = FACE_OUTER_BOUND ( 'NONE', #6813, .T. ) ;
#3775 = DIRECTION ( 'NONE',  ( -5.440186201345738641E-18, -1.000000000000000000, -1.334940939666364181E-17 ) ) ;
#3776 = ORIENTED_EDGE ( 'NONE', *, *, #14294, .F. ) ;
#3777 = ORIENTED_EDGE ( 'NONE', *, *, #14978, .T. ) ;
#3778 = DIRECTION ( 'NONE',  ( 0.3102455404053333088, 0.9506564598521396459, 0.000000000000000000 ) ) ;
#3779 = CARTESIAN_POINT ( 'NONE',  ( -52.56676294784124792, 113.4816418249608034, -43.51333844217711544 ) ) ;
#3780 = ORIENTED_EDGE ( 'NONE', *, *, #17199, .T. ) ;
#3781 = CARTESIAN_POINT ( 'NONE',  ( -49.12744300538584952, 95.04215844998273610, -43.53116934361613488 ) ) ;
#3782 = ORIENTED_EDGE ( 'NONE', *, *, #8180, .F. ) ;
#3783 = DIRECTION ( 'NONE',  ( 0.000000000000000000, 0.000000000000000000, -1.000000000000000000 ) ) ;
#3784 =( LENGTH_UNIT ( ) NAMED_UNIT ( * ) SI_UNIT ( .MILLI., .METRE. ) );
#3785 = DIRECTION ( 'NONE',  ( 0.000000000000000000, 0.000000000000000000, 1.000000000000000000 ) ) ;
#3786 = DIRECTION ( 'NONE',  ( 7.125109674403838460E-05, -0.9999848031710254492, 0.005512562950847868688 ) ) ;
#3787 = CARTESIAN_POINT ( 'NONE',  ( 88.82263333796723259, 169.9999999999999716, -1.148052203164690033 ) ) ;
#3788 = VECTOR ( 'NONE', #18661, 1000.000000000000000 ) ;
#3789 = AXIS2_PLACEMENT_3D ( 'NONE', #15759, #10684, #5378 ) ;
#3790 = ORIENTED_EDGE ( 'NONE', *, *, #16760, .F. ) ;
#3791 = EDGE_CURVE ( 'NONE', #19957, #16597, #6318, .T. ) ;
#3792 = CARTESIAN_POINT ( 'NONE',  ( 37.74318974735589904, 93.98903733564172569, 82.45639132626887147 ) ) ;
#3793 = CARTESIAN_POINT ( 'NONE',  ( -5.563703806604332058, 326.7005119474492290, 320.3383740725300299 ) ) ;
#3794 = VERTEX_POINT ( 'NONE', #1304 ) ;
#3795 = AXIS2_PLACEMENT_3D ( 'NONE', #226, #9614, #22431 ) ;
#3796 = DIRECTION ( 'NONE',  ( 7.125109674070808144E-05, -0.9999848031710253382, 0.005512562950849314580 ) ) ;
#3797 = CARTESIAN_POINT ( 'NONE',  ( -90.07961787348274640, 87.54157812894763424, 51.06841591324713647 ) ) ;
#3798 = ADVANCED_FACE ( 'NONE', ( #6671 ), #14248, .T. ) ;
#3799 = B_SPLINE_CURVE_WITH_KNOTS ( 'NONE', 3,
 ( #6965, #5005, #15388, #10311, #12034, #20404, #15613, #6522, #6850, #19023, #13539, #3286, #13872, #11823 ),
 .UNSPECIFIED., .F., .F.,
 ( 4, 2, 2, 2, 2, 2, 4 ),
 ( 0.05403846203490970945, 0.06102746434071360665, 0.06801646664651750385, 0.08199447125812529824, 0.08898347356392918850, 0.09597247586973307876, 0.1099504804813408732 ),
 .UNSPECIFIED. ) ;
#3800 = AXIS2_PLACEMENT_3D ( 'NONE', #16016, #7026, #366 ) ;
#3801 = ORIENTED_EDGE ( 'NONE', *, *, #16971, .T. ) ;
#3802 = AXIS2_PLACEMENT_3D ( 'NONE', #10510, #7274, #7170 ) ;
#3803 = ORIENTED_EDGE ( 'NONE', *, *, #19177, .F. ) ;
#3804 = DIRECTION ( 'NONE',  ( -0.01292394549866745720, -0.005513023399720816918, -0.9999012842304692006 ) ) ;
#3805 = FACE_OUTER_BOUND ( 'NONE', #17227, .T. ) ;
#3806 = ORIENTED_EDGE ( 'NONE', *, *, #15296, .F. ) ;
#3807 = DIRECTION ( 'NONE',  ( -0.2126763768167737323, -0.9770888199431678744, 0.008136134595576589509 ) ) ;
#3808 = DIRECTION ( 'NONE',  ( 0.01292394549866731669, 0.005513023399720593139, 0.9999012842304692006 ) ) ;
#3809 = ORIENTED_EDGE ( 'NONE', *, *, #2794, .F. ) ;
#3810 = LINE ( 'NONE', #19544, #8762 ) ;
#3811 = VERTEX_POINT ( 'NONE', #17246 ) ;
#3812 = CYLINDRICAL_SURFACE ( 'NONE', #21633, 2.000000000000004885 ) ;
#3813 = LINE ( 'NONE', #17857, #9697 ) ;
#3814 = VECTOR ( 'NONE', #13690, 1000.000000000000000 ) ;
#3815 = CARTESIAN_POINT ( 'NONE',  ( -75.31779428286061773, 75.02317907734844482, 3.077797884313373977 ) ) ;
#3816 = CIRCLE ( 'NONE', #16679, 8.000000000000003553 ) ;
#3817 = CARTESIAN_POINT ( 'NONE',  ( -23.03053847350000538, 324.7037969250150695, 320.5318774195161495 ) ) ;
#3818 = CYLINDRICAL_SURFACE ( 'NONE', #15091, 2.999999999999988898 ) ;
#3819 = ORIENTED_EDGE ( 'NONE', *, *, #16193, .F. ) ;
#3820 = EDGE_CURVE ( 'NONE', #12, #3588, #6460, .T. ) ;
#3821 = CARTESIAN_POINT ( 'NONE',  ( -73.00030478232707765, 95.66452290628956234, 82.28581592040848136 ) ) ;
#3822 = EDGE_CURVE ( 'NONE', #1653, #16867, #6535, .T. ) ;
#3823 = AXIS2_PLACEMENT_3D ( 'NONE', #13459, #3282, #15074 ) ;
#3824 = DIRECTION ( 'NONE',  ( 0.01246513159389404414, 0.2641402835564772844, 0.9644037178988117409 ) ) ;
#3825 = ORIENTED_EDGE ( 'NONE', *, *, #2315, .T. ) ;
#3826 = TOROIDAL_SURFACE ( 'NONE', #20309, 25.26969600708473607, 3.000000000000000000 ) ;
#3827 = CARTESIAN_POINT ( 'NONE',  ( 58.10057221494500368, 126.2575686056377435, 46.09355478759161429 ) ) ;
#3828 = VERTEX_POINT ( 'NONE', #2785 ) ;
#3829 = ORIENTED_EDGE ( 'NONE', *, *, #21301, .T. ) ;
#3830 = ORIENTED_EDGE ( 'NONE', *, *, #7238, .F. ) ;
#3831 = APPLICATION_CONTEXT ( 'automotive_design' ) ;
#3832 = DIRECTION ( 'NONE',  ( 1.000000000000000000, 0.000000000000000000, -1.387778780781445833E-14 ) ) ;
#3833 = AXIS2_PLACEMENT_3D ( 'NONE', #14116, #20862, #17680 ) ;
#3835 = ORIENTED_EDGE ( 'NONE', *, *, #3149, .T. ) ;
#3834 = ORIENTED_EDGE ( 'NONE', *, *, #17947, .F. ) ;
#3836 = CARTESIAN_POINT ( 'NONE',  ( 17.14183078491316436, 175.4877217292663545, 88.23789649046089778 ) ) ;
#3837 = DIRECTION ( 'NONE',  ( 0.9250486434174661765, 0.3795887553195633202, -0.01404934683357507604 ) ) ;
#3838 = CARTESIAN_POINT ( 'NONE',  ( -91.70242328196546566, 70.02268785600074352, 60.75168657352403301 ) ) ;
#3839 = AXIS2_PLACEMENT_3D ( 'NONE', #2722, #6603, #10070 ) ;
#3840 = CARTESIAN_POINT ( 'NONE',  ( 1.364374644014609697E-14, 69.99999999999998579, -9.836443712999143722E-15 ) ) ;
#3841 = DIRECTION ( 'NONE',  ( -2.025474946048326158E-22, 1.000000000000000000, -1.876735158486679638E-22 ) ) ;
#3842 = ORIENTED_EDGE ( 'NONE', *, *, #8919, .F. ) ;
#3843 = CARTESIAN_POINT ( 'NONE',  ( 75.23002811022017511, 75.08930679774387329, -5.101340048736655142 ) ) ;
#3844 = CARTESIAN_POINT ( 'NONE',  ( 19.21689716288775074, 184.4993076657424353, 311.6842248372922199 ) ) ;
#3845 = DIRECTION ( 'NONE',  ( 0.9998688410312766006, 0.009690170827377627902, -0.01297695357578096571 ) ) ;
#3846 = DIRECTION ( 'NONE',  ( 7.125109674364534776E-05, -0.9999848031710252272, 0.005512562950849704893 ) ) ;
#3847 =( NAMED_UNIT ( * ) SI_UNIT ( $, .STERADIAN. ) SOLID_ANGLE_UNIT ( ) );
#3848 = MECHANICAL_DESIGN_GEOMETRIC_PRESENTATION_REPRESENTATION (  '', ( #6432 ), #20715 ) ;
#3849 = CARTESIAN_POINT ( 'NONE',  ( -16.67992392942989710, 141.4150907639733248, 256.9972695922879780 ) ) ;
#3850 = DIRECTION ( 'NONE',  ( -7.125109674160258889E-05, 0.9999848031710252272, -0.005512562950849896580 ) ) ;
#3851 = ORIENTED_EDGE ( 'NONE', *, *, #11320, .F. ) ;
#3852 = CARTESIAN_POINT ( 'NONE',  ( -66.32153322427998887, 169.4339520569534159, -101.8244805435235918 ) ) ;
#3853 = ORIENTED_EDGE ( 'NONE', *, *, #2422, .T. ) ;
#3854 = EDGE_LOOP ( 'NONE', ( #15281, #11812, #16723 ) ) ;
#3855 = CARTESIAN_POINT ( 'NONE',  ( 106.9749367633763910, 184.8436277385793289, 25.61958048976753943 ) ) ;
#3856 = ADVANCED_FACE ( 'NONE', ( #15428 ), #18372, .F. ) ;
#3857 = PRESENTATION_STYLE_ASSIGNMENT (( #19585 ) ) ;
#3858 = CIRCLE ( 'NONE', #4941, 2.000000000000005773 ) ;
#3859 = ORIENTED_EDGE ( 'NONE', *, *, #8501, .T. ) ;
#3860 = DIRECTION ( 'NONE',  ( -0.01292394549866741384, -0.005513023399720269613, -0.9999012842304692006 ) ) ;
#3861 = CARTESIAN_POINT ( 'NONE',  ( -16.67992392942989710, 141.4150907639733248, 256.9972695922879780 ) ) ;
#3862 = ORIENTED_EDGE ( 'NONE', *, *, #3596, .F. ) ;
#3863 = CARTESIAN_POINT ( 'NONE',  ( -6.855465143029762842, 165.4878681845327151, 88.60220162439657088 ) ) ;
#3864 = VERTEX_POINT ( 'NONE', #1250 ) ;
#3865 = CARTESIAN_POINT ( 'NONE',  ( -55.02204129777265962, 114.2332515310180980, 162.5539611862375011 ) ) ;
#3866 = CARTESIAN_POINT ( 'NONE',  ( 67.43998885458336190, 192.1904093341285886, 33.60813087397579579 ) ) ;
#3867 = CARTESIAN_POINT ( 'NONE',  ( -91.28310237474858013, 79.93543901797764306, 31.44354501024113446 ) ) ;
#3868 = CARTESIAN_POINT ( 'NONE',  ( 1.247179693797900502, 69.99999999999998579, 96.49194029975444664 ) ) ;
#3869 = EDGE_LOOP ( 'NONE', ( #14299, #3213, #506 ) ) ;
#3870 = EDGE_CURVE ( 'NONE', #18167, #12292, #22291, .T. ) ;
#3871 = CARTESIAN_POINT ( 'NONE',  ( -13.02223955641218822, 183.9466781734064114, 319.8591424033813837 ) ) ;
#3872 = EDGE_CURVE ( 'NONE', #3975, #8205, #20298, .T. ) ;
#3873 = ORIENTED_EDGE ( 'NONE', *, *, #532, .F. ) ;
#3874 = CARTESIAN_POINT ( 'NONE',  ( 92.82229925712805141, 72.00000000000000000, -1.199748770783255924 ) ) ;
#3875 = CARTESIAN_POINT ( 'NONE',  ( -5.860583941020064636, 326.6140704304781366, 307.3310200717714338 ) ) ;
#3876 = CARTESIAN_POINT ( 'NONE',  ( -13.61876686344269416, 180.6360036619030893, 319.1235917264722275 ) ) ;
#3877 = PLANE ( 'NONE',  #17995 ) ;
#3878 = ORIENTED_EDGE ( 'NONE', *, *, #3762, .T. ) ;
#3879 = PLANE ( 'NONE',  #17324 ) ;
#3880 = ADVANCED_FACE ( 'NONE', ( #13526 ), #20839, .T. ) ;
#3881 = EDGE_CURVE ( 'NONE', #20719, #7056, #6943, .T. ) ;
#3882 = CARTESIAN_POINT ( 'NONE',  ( -42.56847267762256593, 125.7553391191873544, -43.71024041842355246 ) ) ;
#3883 = EDGE_CURVE ( 'NONE', #5147, #14492, #21904, .T. ) ;
#3884 = CARTESIAN_POINT ( 'NONE',  ( -56.11570452959804101, 145.0902203831569466, 107.4719138853213991 ) ) ;
#3885 = CYLINDRICAL_SURFACE ( 'NONE', #15169, 7.999999999999985789 ) ;
#3886 = ORIENTED_EDGE ( 'NONE', *, *, #12455, .T. ) ;
#3887 = ORIENTED_EDGE ( 'NONE', *, *, #18824, .T. ) ;
#3888 = PLANE ( 'NONE',  #10914 ) ;
#3889 = EDGE_LOOP ( 'NONE', ( #10296, #14339, #7819, #3948 ) ) ;
#3890 = ORIENTED_EDGE ( 'NONE', *, *, #6561, .F. ) ;
#3891 = DIRECTION ( 'NONE',  ( -0.7070981056135072773, 0.7070960354057256314, 0.005240777737525932969 ) ) ;
#3892 = DIRECTION ( 'NONE',  ( 5.440186201345810285E-18, 1.000000000000000000, 1.334940939666369727E-17 ) ) ;
#3893 = CARTESIAN_POINT ( 'NONE',  ( 55.40268456415105902, 20.00000000000000000, -113.1659955246503699 ) ) ;
#3894 = CARTESIAN_POINT ( 'NONE',  ( -5.193835686285779296, 86.33565059398134167, 75.28338189912726364 ) ) ;
#3895 = EDGE_CURVE ( 'NONE', #9274, #18312, #1772, .T. ) ;
#3896 = CARTESIAN_POINT ( 'NONE',  ( 19.85551708207331245, 148.5512754185721462, 278.3770131723069312 ) ) ;
#3897 = CARTESIAN_POINT ( 'NONE',  ( -8.515086503764345949, 185.4173453262823728, 305.3464451745876431 ) ) ;
#3898 = ORIENTED_EDGE ( 'NONE', *, *, #5677, .F. ) ;
#3899 = CYLINDRICAL_SURFACE ( 'NONE', #3982, 2.000000000000001332 ) ;
#3900 = CARTESIAN_POINT ( 'NONE',  ( -89.98474239258742102, 87.74831365670060279, 50.94151585748681299 ) ) ;
#3901 = DIRECTION ( 'NONE',  ( 0.3957342950827466566, 0.000000000000000000, 0.9183650514339936066 ) ) ;
#3903 = ORIENTED_EDGE ( 'NONE', *, *, #3283, .F. ) ;
#3902 = ORIENTED_EDGE ( 'NONE', *, *, #93, .T. ) ;
#3904 = EDGE_CURVE ( 'NONE', #13498, #10132, #10180, .T. ) ;
#3905 = ORIENTED_EDGE ( 'NONE', *, *, #5439, .T. ) ;
#3906 = LINE ( 'NONE', #14270, #21683 ) ;
#3907 = CARTESIAN_POINT ( 'NONE',  ( -64.99457118636313169, 170.0000000000000284, 0.8400692238016805868 ) ) ;
#3908 = CARTESIAN_POINT ( 'NONE',  ( 153.9999999999992610, 18.00000000000000355, -53.76161406891471017 ) ) ;
#3909 = DIRECTION ( 'NONE',  ( 0.01292394549866738608, 0.005513023399720698957, 0.9999012842304692006 ) ) ;
#3910 = DIRECTION ( 'NONE',  ( 0.2317097747526812579, -0.9727820773532223075, 0.002368599673008277024 ) ) ;
#3911 = ORIENTED_EDGE ( 'NONE', *, *, #6131, .F. ) ;
#3912 = DIRECTION ( 'NONE',  ( -0.01292414190464131508, 0.000000000000000000, -0.9999164797902017066 ) ) ;
#3913 = ORIENTED_EDGE ( 'NONE', *, *, #21314, .T. ) ;
#3914 = CARTESIAN_POINT ( 'NONE',  ( -164.0000000000000000, 18.00000000000000355, 8.000000000000019540 ) ) ;
#3915 = CARTESIAN_POINT ( 'NONE',  ( -92.91906646248267521, 77.13883058002311088, -28.81763569833110239 ) ) ;
#3916 = CARTESIAN_POINT ( 'NONE',  ( -74.93482218714731857, 75.00176059250013338, 0.3029847661794342062 ) ) ;
#3917 = CARTESIAN_POINT ( 'NONE',  ( -10.18122515959160701, 165.1294603137475860, 320.6223196198712913 ) ) ;
#3918 = CARTESIAN_POINT ( 'NONE',  ( 4.376210989365964643, 95.03750572909316929, -92.29796090835097289 ) ) ;
#3919 = EDGE_CURVE ( 'NONE', #5652, #22611, #12407, .T. ) ;
#3920 = DIRECTION ( 'NONE',  ( 0.9999164797902017066, 6.965998958219367529E-18, -0.01292414190464157182 ) ) ;
#3921 = CARTESIAN_POINT ( 'NONE',  ( 65.91132296857659867, 106.8060942374655156, 70.08728685723174578 ) ) ;
#3922 = LINE ( 'NONE', #7604, #13 ) ;
#3923 = EDGE_LOOP ( 'NONE', ( #16079, #13807, #18487, #11398, #15466, #9182, #3853, #7722, #17575, #5613 ) ) ;
#3924 = FACE_BOUND ( 'NONE', #15682, .T. ) ;
#3925 = ORIENTED_EDGE ( 'NONE', *, *, #14030, .F. ) ;
#3926 = ORIENTED_EDGE ( 'NONE', *, *, #17629, .T. ) ;
#3927 = CARTESIAN_POINT ( 'NONE',  ( -84.09223301484821889, 75.05036917497851334, -2.018900408767783983 ) ) ;
#3928 = CARTESIAN_POINT ( 'NONE',  ( 16.39634482804422433, 187.9401017119210451, 319.7988598509798521 ) ) ;
#3929 = VECTOR ( 'NONE', #19088, 999.9999999999998863 ) ;
#3930 = EDGE_CURVE ( 'NONE', #2309, #13637, #6615, .T. ) ;
#3931 = CARTESIAN_POINT ( 'NONE',  ( 93.23587179807657321, 72.00000000000000000, 30.79757858250317071 ) ) ;
#3932 = EDGE_CURVE ( 'NONE', #10181, #14619, #17188, .T. ) ;
#3933 = CARTESIAN_POINT ( 'NONE',  ( -10.82553926660208354, 163.7173592118130045, 130.2889465353590310 ) ) ;
#3934 = DIRECTION ( 'NONE',  ( 0.01292394549866738608, 0.005513023399720468239, 0.9999012842304692006 ) ) ;
#3935 = CARTESIAN_POINT ( 'NONE',  ( -7.475646132950445555, 81.99999999999998579, -81.73701953211951832 ) ) ;
#3936 = DIRECTION ( 'NONE',  ( -0.01292394549866733230, -0.005513023399720419666, -0.9999012842304692006 ) ) ;
#3937 = VERTEX_POINT ( 'NONE', #13857 ) ;
#3938 = CARTESIAN_POINT ( 'NONE',  ( -10.80367058494921118, 137.7226637369942068, 131.3225862426590709 ) ) ;
#3939 = CARTESIAN_POINT ( 'NONE',  ( 20.36241020427591408, 184.0347753543214537, 278.2158687833079966 ) ) ;
#3940 = CARTESIAN_POINT ( 'NONE',  ( 18.61482433265386405, 185.2913030115592221, 310.7831755306406762 ) ) ;
#3941 = CARTESIAN_POINT ( 'NONE',  ( 91.47552206421229926, 77.76803451549852753, 29.83954006679655535 ) ) ;
#3942 = DIRECTION ( 'NONE',  ( 2.025474946048326158E-22, -1.000000000000000000, 1.876735158486679638E-22 ) ) ;
#3943 = CONICAL_SURFACE ( 'NONE', #16814, 9.000000000000001776, 1.047197551196594301 ) ;
#3944 = CARTESIAN_POINT ( 'NONE',  ( -35.41655530694463749, 106.0996895337223407, 200.1218115885957332 ) ) ;
#3945 = DIRECTION ( 'NONE',  ( -0.9999164797902015955, -2.457859219970326020E-15, 0.01292414190464043211 ) ) ;
#3946 = EDGE_LOOP ( 'NONE', ( #5781, #16810, #11865, #8078 ) ) ;
#3947 = CARTESIAN_POINT ( 'NONE',  ( -90.70439626174763248, 79.29995750804913257, -27.08818539008188964 ) ) ;
#3948 = ORIENTED_EDGE ( 'NONE', *, *, #14878, .T. ) ;
#3949 = VECTOR ( 'NONE', #5099, 1000.000000000000114 ) ;
#3950 = DIRECTION ( 'NONE',  ( -0.01292394549866739996, -0.005513023399721131770, -0.9999012842304692006 ) ) ;
#3951 = DIRECTION ( 'NONE',  ( 7.125109674364534776E-05, -0.9999848031710252272, 0.005512562950849704893 ) ) ;
#3952 =( NAMED_UNIT ( * ) SI_UNIT ( $, .STERADIAN. ) SOLID_ANGLE_UNIT ( ) );
#3953 = VERTEX_POINT ( 'NONE', #8439 ) ;
#3954 = CARTESIAN_POINT ( 'NONE',  ( 13.76243855136152838, 137.5384677217048193, 97.59171006575670049 ) ) ;
#3955 = CARTESIAN_POINT ( 'NONE',  ( 78.64967525538004622, 75.19535340807551904, 5.073326618873633009 ) ) ;
#3956 = FACE_OUTER_BOUND ( 'NONE', #2161, .T. ) ;
#3957 = ORIENTED_EDGE ( 'NONE', *, *, #10582, .F. ) ;
#3958 = CARTESIAN_POINT ( 'NONE',  ( 12.98486085753333263, 190.3233720689114818, 320.8552415163618434 ) ) ;
#3959 = DIRECTION ( 'NONE',  ( 0.6179947723592160713, 1.257324769911454700E-17, -0.7861822061943918305 ) ) ;
#3960 = LINE ( 'NONE', #4080, #21766 ) ;
#3961 = CARTESIAN_POINT ( 'NONE',  ( 51.90570505437388249, 106.9898499841750521, 70.07644525255086876 ) ) ;
#3962 = PRESENTATION_STYLE_ASSIGNMENT (( #9022 ) ) ;
#3963 = CARTESIAN_POINT ( 'NONE',  ( -91.57356387979842793, 79.88289403011208378, 31.31484984389048876 ) ) ;
#3964 = FACE_OUTER_BOUND ( 'NONE', #19952, .T. ) ;
#3965 = ORIENTED_EDGE ( 'NONE', *, *, #10786, .F. ) ;
#3966 = AXIS2_PLACEMENT_3D ( 'NONE', #15003, #2362, #21955 ) ;
#3967 = DIRECTION ( 'NONE',  ( 0.4397038457472424167, 0.000000000000000000, -0.8981428216242032248 ) ) ;
#3968 = ORIENTED_EDGE ( 'NONE', *, *, #2935, .T. ) ;
#3969 = DIRECTION ( 'NONE',  ( -0.009088227368120585167, -0.7109943316365089361, -0.7031390079522393810 ) ) ;
#3970 = CARTESIAN_POINT ( 'NONE',  ( -15.08775915360043207, 178.5843476654970914, 314.2199384936897104 ) ) ;
#3971 = VECTOR ( 'NONE', #2005, 1000.000000000000000 ) ;
#3972 = ORIENTED_EDGE ( 'NONE', *, *, #21272, .F. ) ;
#3973 = ORIENTED_EDGE ( 'NONE', *, *, #18882, .F. ) ;
#3974 = CARTESIAN_POINT ( 'NONE',  ( 39.42082737383937996, 72.00000000000000000, -83.51645567887783272 ) ) ;
#3975 = VERTEX_POINT ( 'NONE', #15596 ) ;
#3976 = ADVANCED_FACE ( 'NONE', ( #6730 ), #9095, .T. ) ;
#3977 = CARTESIAN_POINT ( 'NONE',  ( 12.15711459821606155, 188.6915557983204224, 307.0876295708031876 ) ) ;
#3978 = CIRCLE ( 'NONE', #18301, 3.399999999999986144 ) ;
#3979 = EDGE_CURVE ( 'NONE', #1930, #1614, #16828, .T. ) ;
#3980 = EDGE_LOOP ( 'NONE', ( #15650, #18663, #20093, #5836, #16555 ) ) ;
#3981 = CARTESIAN_POINT ( 'NONE',  ( -4.905708827035320851, 164.7686025659857023, 81.69904712205610053 ) ) ;
#3982 = AXIS2_PLACEMENT_3D ( 'NONE', #9058, #11260, #18269 ) ;
#3983 = CARTESIAN_POINT ( 'NONE',  ( 2.830031787867828275, 81.19615242270661781, -80.39798906481894392 ) ) ;
#3984 = VERTEX_POINT ( 'NONE', #7286 ) ;
#3985 = DIRECTION ( 'NONE',  ( -0.01104128644981183967, -0.5197558313507629757, -0.8542435049623791077 ) ) ;
#3986 = EDGE_LOOP ( 'NONE', ( #2523, #7255, #6886, #20344, #9961, #387, #15871, #9783, #1127, #16837, #6587, #7019, #22448, #19886, #11056, #14840, #15036, #16890, #18983, #21776, #10606, #17366, #8330, #18255, #14892, #13139, #7663, #4579, #2706, #13194, #16010, #2732, #10375, #5309, #14590, #13641 ) ) ;
#3987 = CARTESIAN_POINT ( 'NONE',  ( -13.92525281995234820, 325.7770340667113942, 328.4523304068723064 ) ) ;
#3988 = ORIENTED_EDGE ( 'NONE', *, *, #5250, .F. ) ;
#3989 = FACE_OUTER_BOUND ( 'NONE', #10763, .T. ) ;
#3990 = FACE_OUTER_BOUND ( 'NONE', #15488, .T. ) ;
#3991 = CARTESIAN_POINT ( 'NONE',  ( -42.01023468938293348, 95.04007470540923919, -43.47457758741172285 ) ) ;
#3992 = FACE_BOUND ( 'NONE', #2750, .T. ) ;
#3993 = ADVANCED_FACE ( 'NONE', ( #529 ), #9240, .F. ) ;
#3994 = ORIENTED_EDGE ( 'NONE', *, *, #17938, .T. ) ;
#3995 = ORIENTED_EDGE ( 'NONE', *, *, #10783, .T. ) ;
#3996 = CARTESIAN_POINT ( 'NONE',  ( 17.14183078491316436, 175.4877217292663545, 88.23789649046089778 ) ) ;
#3997 = VECTOR ( 'NONE', #13077, 1000.000000000000114 ) ;
#3998 = COLOUR_RGB ( '', 0.72549020, 0.75294118, 0.79215686) ;
#3999 = CARTESIAN_POINT ( 'NONE',  ( -3.030255530017816668, 323.0571258370100054, 414.2134192087003726 ) ) ;
#4000 = EDGE_CURVE ( 'NONE', #16185, #5296, #21189, .T. ) ;
#4001 = AXIS2_PLACEMENT_3D ( 'NONE', #2856, #15179, #18821 ) ;
#4002 = ORIENTED_EDGE ( 'NONE', *, *, #21675, .T. ) ;
#4003 = DIRECTION ( 'NONE',  ( -2.025474946048326158E-22, 1.000000000000000000, -1.876735158486679638E-22 ) ) ;
#4004 = CARTESIAN_POINT ( 'NONE',  ( -89.40021307249486426, 89.12052993720315897, 51.52924698431865380 ) ) ;
#4005 = SHAPE_DEFINITION_REPRESENTATION ( #13997, #11808 ) ;
#4006 = EDGE_CURVE ( 'NONE', #21984, #22611, #14328, .T. ) ;
#4007 = EDGE_LOOP ( 'NONE', ( #16383, #13424 ) ) ;
#4008 = EDGE_CURVE ( 'NONE', #2673, #16531, #9469, .T. ) ;
#4009 = CARTESIAN_POINT ( 'NONE',  ( -2.322807172541347498, 81.99999999999998579, -81.06750429846923112 ) ) ;
#4010 = EDGE_LOOP ( 'NONE', ( #2428, #19590, #9387, #16670 ) ) ;
#4011 = LINE ( 'NONE', #16357, #14018 ) ;
#4012 = ADVANCED_FACE ( 'NONE', ( #16170 ), #7410, .F. ) ;
#4013 = DIRECTION ( 'NONE',  ( 0.000000000000000000, 0.000000000000000000, 1.000000000000000000 ) ) ;
#4014 = ADVANCED_FACE ( 'NONE', ( #9819 ), #10214, .F. ) ;
#4015 = CARTESIAN_POINT ( 'NONE',  ( -105.9930786687657189, 70.38870405239201489, -29.41946405304836887 ) ) ;
#4016 = AXIS2_PLACEMENT_3D ( 'NONE', #179, #281, #5209 ) ;
#4017 = CARTESIAN_POINT ( 'NONE',  ( 14.04531128256715888, 105.6586476617446380, 119.4770396839737714 ) ) ;
#4018 = ORIENTED_EDGE ( 'NONE', *, *, #20003, .F. ) ;
#4019 = DIRECTION ( 'NONE',  ( -0.8637520339192008567, -0.002839416958727990648, -0.5039090806998601790 ) ) ;
#4020 = VERTEX_POINT ( 'NONE', #14790 ) ;
#4021 = DIRECTION ( 'NONE',  ( 0.9999164797902015955, 2.001050586450178695E-22, -0.01292414190464131335 ) ) ;
#4022 = VECTOR ( 'NONE', #7656, 999.9999999999998863 ) ;
#4023 = DIRECTION ( 'NONE',  ( 0.01292394549866738088, 0.005513023399720295634, 0.9999012842304693116 ) ) ;
#4024 = DIRECTION ( 'NONE',  ( 0.000000000000000000, 1.000000000000000000, -0.000000000000000000 ) ) ;
#4025 = CARTESIAN_POINT ( 'NONE',  ( 3.575103298931712636, 166.5249713112435188, 276.5989983650335375 ) ) ;
#4026 = CARTESIAN_POINT ( 'NONE',  ( 45.34010913598296355, 168.6466622724117599, 26.02279695137911020 ) ) ;
#4027 = ORIENTED_EDGE ( 'NONE', *, *, #13075, .F. ) ;
#4028 = CARTESIAN_POINT ( 'NONE',  ( -37.51330139321489554, 72.00000000000000000, 87.03232607370787832 ) ) ;
#4029 = FACE_BOUND ( 'NONE', #2296, .T. ) ;
#4030 = AXIS2_PLACEMENT_3D ( 'NONE', #7902, #20062, #14938 ) ;
#4031 = CARTESIAN_POINT ( 'NONE',  ( -50.76769345292276370, 109.8130285628466538, -46.02948977673421638 ) ) ;
#4032 = ORIENTED_EDGE ( 'NONE', *, *, #3791, .F. ) ;
#4033 = DIRECTION ( 'NONE',  ( -7.125109674160325297E-05, 0.9999848031710253382, -0.005512562950849328458 ) ) ;
#4034 = EDGE_LOOP ( 'NONE', ( #12480, #18041, #19764, #20158 ) ) ;
#4035 = ADVANCED_FACE ( 'NONE', ( #16626 ), #16109, .T. ) ;
#4036 = ORIENTED_EDGE ( 'NONE', *, *, #10468, .T. ) ;
#4037 = VERTEX_POINT ( 'NONE', #11550 ) ;
#4038 = AXIS2_PLACEMENT_3D ( 'NONE', #9351, #13057, #2804 ) ;
#4039 = CARTESIAN_POINT ( 'NONE',  ( -82.19103547355555861, 75.11063986505352830, 5.648077914104375985 ) ) ;
#4040 = VECTOR ( 'NONE', #34, 999.9999999999998863 ) ;
#4041 = FACE_OUTER_BOUND ( 'NONE', #14264, .T. ) ;
#4042 = CARTESIAN_POINT ( 'NONE',  ( -146.5000000000000000, 1.999999999999998224, -7.999999999999981348 ) ) ;
#4044 = ORIENTED_EDGE ( 'NONE', *, *, #4897, .T. ) ;
#4043 = VERTEX_POINT ( 'NONE', #18439 ) ;
#4045 = ADVANCED_FACE ( 'NONE', ( #6254 ), #17189, .T. ) ;
#4046 = VECTOR ( 'NONE', #5440, 1000.000000000000114 ) ;
#4047 = CARTESIAN_POINT ( 'NONE',  ( 39.80634724086582565, 95.47920460943406340, -43.77198102653553491 ) ) ;
#4048 = CARTESIAN_POINT ( 'NONE',  ( -10.05852611029434307, 146.4821163384300462, 278.3017991042662516 ) ) ;
#4049 = CARTESIAN_POINT ( 'NONE',  ( 2.924639046024143596, 174.5833632305869401, 296.5649497806293766 ) ) ;
#4050 = CARTESIAN_POINT ( 'NONE',  ( 70.71197882986199090, 71.18508886668922742, 84.26048200481866957 ) ) ;
#4051 = CARTESIAN_POINT ( 'NONE',  ( 39.99665919160806027, 170.0000000000000284, -0.5169656761856848970 ) ) ;
#4052 = CARTESIAN_POINT ( 'NONE',  ( -162.0000000000000000, 0.000000000000000000, -53.76161406891256433 ) ) ;
#4053 = CARTESIAN_POINT ( 'NONE',  ( 20.55381086804826651, 182.0128392866518823, 312.7933888596797374 ) ) ;
#4054 = CARTESIAN_POINT ( 'NONE',  ( 7.025502335143726462, 174.6876751029090542, 81.49014409824067684 ) ) ;
#4055 = AXIS2_PLACEMENT_3D ( 'NONE', #6914, #17746, #19651 ) ;
#4056 = LINE ( 'NONE', #18547, #5507 ) ;
#4057 = SHAPE_REPRESENTATION_RELATIONSHIP ( 'NONE' , 'NONE' ,  #15037, #13490 ) ;
#4058 = CARTESIAN_POINT ( 'NONE',  ( 91.59502366432090525, 95.97275144416938986, 60.91270374391774567 ) ) ;
#4059 = VERTEX_POINT ( 'NONE', #13797 ) ;
#4060 = ADVANCED_FACE ( 'NONE', ( #7869 ), #21620, .F. ) ;
#4061 = FACE_OUTER_BOUND ( 'NONE', #17532, .T. ) ;
#4062 = AXIS2_PLACEMENT_3D ( 'NONE', #1434, #12837, #17065 ) ;
#4063 = CARTESIAN_POINT ( 'NONE',  ( -10.02112475001242586, 187.8727749214653784, 308.1601357688390408 ) ) ;
#4064 = ORIENTED_EDGE ( 'NONE', *, *, #13445, .F. ) ;
#4065 = ORIENTED_EDGE ( 'NONE', *, *, #15984, .F. ) ;
#4066 = DIRECTION ( 'NONE',  ( -0.01292414190464023262, 0.000000000000000000, -0.9999164797902017066 ) ) ;
#4067 = CARTESIAN_POINT ( 'NONE',  ( 2.830031787867828275, 70.80384757729338219, -80.39798906481894392 ) ) ;
#4068 = VECTOR ( 'NONE', #20649, 999.9999999999998863 ) ;
#4069 = LINE ( 'NONE', #11098, #16202 ) ;
#4070 = AXIS2_PLACEMENT_3D ( 'NONE', #20213, #13240, #18720 ) ;
#4071 = CARTESIAN_POINT ( 'NONE',  ( -39.66847363096314893, 93.56461422141673268, -82.92963109642393249 ) ) ;
#4072 = CARTESIAN_POINT ( 'NONE',  ( -90.35604405134509420, 70.78363085573803914, 62.83509160642692848 ) ) ;
#4073 = AXIS2_PLACEMENT_3D ( 'NONE', #2669, #21922, #7834 ) ;
#4074 = FACE_OUTER_BOUND ( 'NONE', #20360, .T. ) ;
#4075 = CARTESIAN_POINT ( 'NONE',  ( 163.9999999999998295, 0.8284271247461892917, -8.000000000002268408 ) ) ;
#4076 = DIRECTION ( 'NONE',  ( -0.9999164797902017066, -2.001050586450178931E-22, 0.01292414190464131508 ) ) ;
#4077 = VECTOR ( 'NONE', #17450, 999.9999999999998863 ) ;
#4078 = ORIENTED_EDGE ( 'NONE', *, *, #19331, .T. ) ;
#4079 = DIRECTION ( 'NONE',  ( 0.000000000000000000, 0.000000000000000000, 1.000000000000000000 ) ) ;
#4080 = CARTESIAN_POINT ( 'NONE',  ( -36.79753515562058652, 127.3639955235004777, 248.0271576934996745 ) ) ;
#4081 = CARTESIAN_POINT ( 'NONE',  ( -8.641754912934437982, 185.9330366646549066, 321.2360663095644213 ) ) ;
#4082 = CARTESIAN_POINT ( 'NONE',  ( -92.35396912051191975, 79.82103140542292863, 31.19620131593478618 ) ) ;
#4083 = DIRECTION ( 'NONE',  ( 7.125109674160325297E-05, -0.9999848031710252272, 0.005512562950849327591 ) ) ;
#4084 = EDGE_LOOP ( 'NONE', ( #16353, #17998, #8300 ) ) ;
#4085 = VECTOR ( 'NONE', #15757, 1000.000000000000114 ) ;
#4086 = DIRECTION ( 'NONE',  ( -0.01292394549866745720, -0.005513023399720816918, -0.9999012842304692006 ) ) ;
#4087 = VECTOR ( 'NONE', #1216, 1000.000000000000227 ) ;
#4088 = ORIENTED_EDGE ( 'NONE', *, *, #17676, .F. ) ;
#4089 = ADVANCED_FACE ( 'NONE', ( #21512 ), #20480, .F. ) ;
#4090 = DIRECTION ( 'NONE',  ( -0.9999164797902017066, -6.965998958219365988E-18, 0.01292414190464157356 ) ) ;
#4091 = CARTESIAN_POINT ( 'NONE',  ( -9.868119059700692475, 184.4438714364067380, 308.0446564981782558 ) ) ;
#4092 = EDGE_CURVE ( 'NONE', #822, #10707, #695, .T. ) ;
#4093 = ORIENTED_EDGE ( 'NONE', *, *, #10359, .T. ) ;
#4094 = AXIS2_PLACEMENT_3D ( 'NONE', #12668, #3804, #249 ) ;
#4095 = VERTEX_POINT ( 'NONE', #21847 ) ;
#4096 = CYLINDRICAL_SURFACE ( 'NONE', #14326, 109.9999999999999716 ) ;
#4097 = AXIS2_PLACEMENT_3D ( 'NONE', #21829, #18743, #3007 ) ;
#4098 = FACE_OUTER_BOUND ( 'NONE', #10798, .T. ) ;
#4099 = AXIS2_PLACEMENT_3D ( 'NONE', #10976, #2246, #761 ) ;
#4100 = CIRCLE ( 'NONE', #5567, 20.50000000000000000 ) ;
#4101 = AXIS2_PLACEMENT_3D ( 'NONE', #10906, #16100, #2291 ) ;
#4102 = LINE ( 'NONE', #5479, #3030 ) ;
#4103 = LINE ( 'NONE', #5947, #13948 ) ;
#4104 = ORIENTED_EDGE ( 'NONE', *, *, #9891, .F. ) ;
#4105 = CARTESIAN_POINT ( 'NONE',  ( 1.741331101896219202, 70.07661102881318982, -98.69074884774435930 ) ) ;
#4106 = DIRECTION ( 'NONE',  ( 0.4910069343201003411, -0.004767316193522950878, -0.8711426192914037969 ) ) ;
#4107 = ORIENTED_EDGE ( 'NONE', *, *, #4169, .F. ) ;
#4108 = CIRCLE ( 'NONE', #11476, 102.4713510550357398 ) ;
#4109 = DIRECTION ( 'NONE',  ( 0.8981428216242087759, -0.000000000000000000, -0.4397038457472309259 ) ) ;
#4110 = CARTESIAN_POINT ( 'NONE',  ( 12.38356306630694803, 188.4816022558815973, 321.6789667137223319 ) ) ;
#4111 = DIRECTION ( 'NONE',  ( 0.9934404589540163366, 0.1135548637187051429, -0.01346653032743023309 ) ) ;
#4112 = CARTESIAN_POINT ( 'NONE',  ( -9.622921994803601109, 336.0360340286487713, 414.2270707938455416 ) ) ;
#4113 = ORIENTED_EDGE ( 'NONE', *, *, #17200, .T. ) ;
#4114 = ORIENTED_EDGE ( 'NONE', *, *, #11916, .T. ) ;
#4115 = DIRECTION ( 'NONE',  ( 0.000000000000000000, 1.000000000000000000, -0.000000000000000000 ) ) ;
#4116 = CIRCLE ( 'NONE', #8892, 2.000000000000001776 ) ;
#4117 = ADVANCED_FACE ( 'NONE', ( #4183 ), #5428, .F. ) ;
#4118 = DIRECTION ( 'NONE',  ( 0.9999164797902015955, 2.045145117964614424E-15, -0.01292414190464167591 ) ) ;
#4119 = VERTEX_POINT ( 'NONE', #2586 ) ;
#4120 = FACE_OUTER_BOUND ( 'NONE', #13840, .T. ) ;
#4121 = CARTESIAN_POINT ( 'NONE',  ( -88.60388113770839880, 88.93104369895573313, 50.69025205339234930 ) ) ;
#4122 = AXIS2_PLACEMENT_3D ( 'NONE', #2160, #3775, #223 ) ;
#4123 = ORIENTED_EDGE ( 'NONE', *, *, #10099, .F. ) ;
#4124 = CARTESIAN_POINT ( 'NONE',  ( -64.99457118636311748, 170.0000000000008242, 0.8400692238025471159 ) ) ;
#4125 = EDGE_CURVE ( 'NONE', #4299, #6677, #4288, .T. ) ;
#4126 = CARTESIAN_POINT ( 'NONE',  ( -90.33062630657602199, 70.31405425862645586, 62.77257892026059949 ) ) ;
#4127 = ORIENTED_EDGE ( 'NONE', *, *, #19905, .F. ) ;
#4128 = CARTESIAN_POINT ( 'NONE',  ( 40.58037928852487397, 106.1692389898096280, 199.3935091201308296 ) ) ;
#4129 =( BOUNDED_SURFACE ( )  B_SPLINE_SURFACE ( 3, 2, ( 
 ( #1830, #6997, #6876 ),
 ( #20545, #15417, #8601 ),
 ( #17127, #14023, #8701 ),
 ( #21010, #6659, #13795 ),
 ( #17232, #20778, #5263 ),
 ( #15752, #11849, #12308 ),
 ( #1502, #19169, #5032 ),
 ( #8825, #6547, #12187 ),
 ( #3444, #13687, #10119 ),
 ( #3551, #18839, #20669 ),
 ( #10226, #12067, #4928 ),
 ( #3322, #1393, #15873 ),
 ( #10345, #11960, #10454 ),
 ( #19286, #18941, #13899 ),
 ( #20891, #10565, #2408 ),
 ( #9288, #19398, #17928 ) ),
 .UNSPECIFIED., .F., .F., .T. ) 
 B_SPLINE_SURFACE_WITH_KNOTS ( ( 4, 2, 2, 2, 2, 2, 2, 4 ),
 ( 3, 3 ),
 ( 0.003676974186938495454, 0.005450118764002107562, 0.006336691052533913182, 0.007223263341065719670, 0.008109835629597526158, 0.008996407918129330911, 0.009882980206661137398, 0.01076955249519294389 ),
 ( 0.000000000000000000, 1.000000000000000000 ),
 .UNSPECIFIED. ) 
 GEOMETRIC_REPRESENTATION_ITEM ( )  RATIONAL_B_SPLINE_SURFACE ( (
 ( 1.000000000000000000, 0.7071067811865460184, 1.000000000000000000),
 ( 1.000000000000000000, 0.6815104794066817462, 1.000000000000000000),
 ( 1.000000000000000000, 0.6547843716139309933, 1.000000000000000000),
 ( 1.000000000000000000, 0.6123586760872794521, 1.000000000000000000),
 ( 1.000000000000000000, 0.5978640991518743286, 1.000000000000000000),
 ( 1.000000000000000000, 0.5691342003131903970, 1.000000000000000000),
 ( 1.000000000000000000, 0.5547710840782603681, 1.000000000000000000),
 ( 1.000000000000000000, 0.5262790914882317095, 1.000000000000000000),
 ( 1.000000000000000000, 0.5119733473728251827, 1.000000000000000000),
 ( 1.000000000000000000, 0.4852625026393655450, 1.000000000000000000),
 ( 1.000000000000000000, 0.4728155099288974816, 1.000000000000000000),
 ( 1.000000000000000000, 0.4509953647258624909, 1.000000000000000000),
 ( 1.000000000000000000, 0.4419745220849347622, 1.000000000000000000),
 ( 1.000000000000000000, 0.4295065217292311499, 1.000000000000000000),
 ( 1.000000000000000000, 0.4259886279742503556, 1.000000000000000000),
 ( 1.000000000000000000, 0.4260362065776441831, 1.000000000000000000) ) ) 
 REPRESENTATION_ITEM ( '' )  SURFACE ( )  );
#4130 = DIRECTION ( 'NONE',  ( 0.009088227368120106384, 0.7109943316365106014, 0.7031390079522377157 ) ) ;
#4131 = AXIS2_PLACEMENT_3D ( 'NONE', #8906, #19473, #3745 ) ;
#4132 = CARTESIAN_POINT ( 'NONE',  ( 82.94572876491719171, 105.0000000000000000, -72.24960954674284608 ) ) ;
#4133 = CIRCLE ( 'NONE', #18471, 2.000000000000004885 ) ;
#4134 = CARTESIAN_POINT ( 'NONE',  ( 68.86686855361776338, 91.87224768293377508, -85.77506393453894873 ) ) ;
#4135 = VERTEX_POINT ( 'NONE', #11429 ) ;
#4136 = EDGE_CURVE ( 'NONE', #7130, #10247, #11091, .T. ) ;
#4137 = LINE ( 'NONE', #16125, #20508 ) ;
#4138 = ORIENTED_EDGE ( 'NONE', *, *, #21939, .F. ) ;
#4139 = LINE ( 'NONE', #14630, #1853 ) ;
#4140 = CARTESIAN_POINT ( 'NONE',  ( 5.149300590115022835, 81.19615242270661781, -98.24794683011701579 ) ) ;
#4141 = DIRECTION ( 'NONE',  ( 0.000000000000000000, 0.000000000000000000, -1.000000000000000000 ) ) ;
#4142 = CARTESIAN_POINT ( 'NONE',  ( -7.939077925311260664, 165.3359731837102515, 308.2574871822228033 ) ) ;
#4143 = CARTESIAN_POINT ( 'NONE',  ( -41.41899454747574083, 166.0889136240115249, 277.1829612759436827 ) ) ;
#4144 = VERTEX_POINT ( 'NONE', #18553 ) ;
#4145 = DIRECTION ( 'NONE',  ( -0.01292394549866749710, -0.005513023399720701559, -0.9999012842304693116 ) ) ;
#4146 = DIRECTION ( 'NONE',  ( 0.01292394549866731843, 0.005513023399720594006, 0.9999012842304693116 ) ) ;
#4147 = ADVANCED_BREP_SHAPE_REPRESENTATION ( '', ( #17421, #6292 ), #12539 ) ;
#4148 = CARTESIAN_POINT ( 'NONE',  ( 40.76338182023881984, 106.2626885438830300, 92.18371853433509955 ) ) ;
#4149 = EDGE_CURVE ( 'NONE', #2088, #20616, #18313, .T. ) ;
#4150 = ORIENTED_EDGE ( 'NONE', *, *, #7212, .T. ) ;
#4151 = CARTESIAN_POINT ( 'NONE',  ( 12.82460312764358612, 190.4936219940274498, 307.8489606432475512 ) ) ;
#4152 = EDGE_CURVE ( 'NONE', #18705, #8847, #13279, .T. ) ;
#4153 = CYLINDRICAL_SURFACE ( 'NONE', #21321, 6.000000000000003553 ) ;
#4154 = EDGE_LOOP ( 'NONE', ( #7510, #12307 ) ) ;
#4155 = AXIS2_PLACEMENT_3D ( 'NONE', #3682, #15780, #14403 ) ;
#4156 = ORIENTED_EDGE ( 'NONE', *, *, #11113, .F. ) ;
#4157 = VERTEX_POINT ( 'NONE', #21739 ) ;
#4158 = AXIS2_PLACEMENT_3D ( 'NONE', #12119, #12464, #8882 ) ;
#4159 = CARTESIAN_POINT ( 'NONE',  ( -80.39616048656512248, 75.13699351169601925, -4.061287812893456639 ) ) ;
#4160 = CARTESIAN_POINT ( 'NONE',  ( -90.14105734218799171, 88.27340299027098069, 52.93867176097701588 ) ) ;
#4161 = ORIENTED_EDGE ( 'NONE', *, *, #19027, .F. ) ;
#4162 = EDGE_CURVE ( 'NONE', #8677, #19674, #8360, .T. ) ;
#4163 = CARTESIAN_POINT ( 'NONE',  ( -37.86293061927234049, 105.7860355035395230, 92.52957110793263951 ) ) ;
#4164 = CARTESIAN_POINT ( 'NONE',  ( -90.03465221005033925, 70.01281497139055432, 63.19621350536183968 ) ) ;
#4165 = CARTESIAN_POINT ( 'NONE',  ( -2.652335923087511205, 190.0839019912061758, 274.7308922624509933 ) ) ;
#4166 = VECTOR ( 'NONE', #9917, 1000.000000000000000 ) ;
#4167 = CARTESIAN_POINT ( 'NONE',  ( -89.59766859896278390, 79.73843791202820341, -28.47398564242251240 ) ) ;
#4168 = CARTESIAN_POINT ( 'NONE',  ( 0.000000000000000000, 29.00000000000000355, -101.0000000000000000 ) ) ;
#4169 = EDGE_CURVE ( 'NONE', #9064, #3348, #2508, .T. ) ;
#4170 = PLANE ( 'NONE',  #20897 ) ;
#4171 = DIRECTION ( 'NONE',  ( 7.125109674160325297E-05, -0.9999848031710252272, 0.005512562950849327591 ) ) ;
#4172 = CARTESIAN_POINT ( 'NONE',  ( 19.67111680476709168, 183.8698952613492281, 312.7070380754294661 ) ) ;
#4173 = VECTOR ( 'NONE', #4589, 999.9999999999998863 ) ;
#4174 = CARTESIAN_POINT ( 'NONE',  ( 77.91909412299041549, 100.1635695855007668, -77.84996988984397603 ) ) ;
#4175 = AXIS2_PLACEMENT_3D ( 'NONE', #10513, #3547, #10673 ) ;
#4176 = DIRECTION ( 'NONE',  ( 0.009188991635466048358, -0.7031977391749438810, 0.7109349492407661675 ) ) ;
#4177 = EDGE_CURVE ( 'NONE', #20449, #18377, #1689, .T. ) ;
#4178 = ADVANCED_FACE ( 'NONE', ( #20356 ), #2453, .F. ) ;
#4179 = CARTESIAN_POINT ( 'NONE',  ( -10.85595612533484911, 109.6999345499266525, 127.2773526115149281 ) ) ;
#4180 = DIRECTION ( 'NONE',  ( 0.9935244165829104634, 0.1136188085379686713, 0.000000000000000000 ) ) ;
#4181 = ORIENTED_EDGE ( 'NONE', *, *, #6263, .F. ) ;
#4182 = CIRCLE ( 'NONE', #17051, 3.399999999999991918 ) ;
#4183 = FACE_OUTER_BOUND ( 'NONE', #14885, .T. ) ;
#4184 = ORIENTED_EDGE ( 'NONE', *, *, #864, .F. ) ;
#4185 = CARTESIAN_POINT ( 'NONE',  ( 42.40290194442976457, 106.8542505984647164, 70.43401943659206665 ) ) ;
#4186 = AXIS2_PLACEMENT_3D ( 'NONE', #18068, #5741, #7704 ) ;
#4187 = VECTOR ( 'NONE', #11318, 1000.000000000000114 ) ;
#4188 = CARTESIAN_POINT ( 'NONE',  ( -41.58451242677338655, 92.58578643762699301, -83.88377541325537834 ) ) ;
#4189 = CARTESIAN_POINT ( 'NONE',  ( -88.38923523735466858, 71.30869604672952278, 62.51339856172231890 ) ) ;
#4190 = CARTESIAN_POINT ( 'NONE',  ( 73.97450750257705465, 75.01358823556745392, 0.6626198993681190474 ) ) ;
#4191 = CARTESIAN_POINT ( 'NONE',  ( -37.41653076871853045, 108.0996591400643752, 200.1366347465033186 ) ) ;
#4192 = ADVANCED_FACE ( 'NONE', ( #11192 ), #13145, .T. ) ;
#4193 = VERTEX_POINT ( 'NONE', #2691 ) ;
#4194 = CARTESIAN_POINT ( 'NONE',  ( -68.81222610331992939, 91.74143318381844381, 85.81887827424428394 ) ) ;
#4195 = ORIENTED_EDGE ( 'NONE', *, *, #4444, .F. ) ;
#4196 = DIRECTION ( 'NONE',  ( -0.9999999898465623538, -0.0001425000279054785136, 7.855523124367795924E-07 ) ) ;
#4197 = AXIS2_PLACEMENT_3D ( 'NONE', #7495, #5872, #14526 ) ;
#4198 = CARTESIAN_POINT ( 'NONE',  ( 163.9999999999992610, 18.00000000000000355, 53.76161406891480965 ) ) ;
#4199 = FACE_OUTER_BOUND ( 'NONE', #10592, .T. ) ;
#4200 = DIRECTION ( 'NONE',  ( 0.01292414190464131508, 1.902755938799530474E-22, 0.9999164797902017066 ) ) ;
#4201 = CARTESIAN_POINT ( 'NONE',  ( -92.46788464407291031, 79.04398536104956463, 28.62013883513307633 ) ) ;
#4202 = FILL_AREA_STYLE_COLOUR ( '', #17670 ) ;
#4203 = ORIENTED_EDGE ( 'NONE', *, *, #19091, .F. ) ;
#4204 = FACE_BOUND ( 'NONE', #14450, .T. ) ;
#4205 = AXIS2_PLACEMENT_3D ( 'NONE', #14508, #5729, #11029 ) ;
#4206 = EDGE_CURVE ( 'NONE', #4699, #15373, #9491, .T. ) ;
#4207 = CARTESIAN_POINT ( 'NONE',  ( -1.163172771417702700, 70.69320546282760631, -89.99248318111824574 ) ) ;
#4208 = CARTESIAN_POINT ( 'NONE',  ( -11.50381294012838040, 186.2556874024963065, 308.5302510577426460 ) ) ;
#4209 = VERTEX_POINT ( 'NONE', #18098 ) ;
#4210 = ORIENTED_EDGE ( 'NONE', *, *, #20593, .F. ) ;
#4211 = DIRECTION ( 'NONE',  ( 0.01292414190463830014, 0.000000000000000000, 0.9999164797902017066 ) ) ;
#4212 = COLOUR_RGB ( '', 0.72549020, 0.75294118, 0.79215686) ;
#4213 = CARTESIAN_POINT ( 'NONE',  ( 11.96358776207564567, 188.1236699898683185, 306.3470157435421015 ) ) ;
#4214 = CONTEXT_DEPENDENT_SHAPE_REPRESENTATION ( #4412, #14188 ) ;
#4215 = CARTESIAN_POINT ( 'NONE',  ( -52.93127853433226448, 189.6011917897851333, -71.71522176735570042 ) ) ;
#4216 = ADVANCED_FACE ( 'NONE', ( #11296 ), #317, .T. ) ;
#4217 = ADVANCED_FACE ( 'NONE', ( #9342 ), #967, .F. ) ;
#4218 = CARTESIAN_POINT ( 'NONE',  ( -6.702556532201369599, 81.97459999999998104, -87.68700545388550438 ) ) ;
#4219 = EDGE_LOOP ( 'NONE', ( #3643, #1404, #7748, #17028, #6097, #953, #20286, #4408, #15572 ) ) ;
#4220 = CARTESIAN_POINT ( 'NONE',  ( -44.26142469380095434, 168.8134312302532862, 57.43298357076854899 ) ) ;
#4221 = VERTEX_POINT ( 'NONE', #18205 ) ;
#4222 = CARTESIAN_POINT ( 'NONE',  ( -12.34320795831280826, 182.0705588102794650, 322.4648799061273508 ) ) ;
#4223 = ORIENTED_EDGE ( 'NONE', *, *, #7186, .F. ) ;
#4224 = ORIENTED_EDGE ( 'NONE', *, *, #19331, .F. ) ;
#4225 = LINE ( 'NONE', #11478, #10713 ) ;
#4226 = ORIENTED_EDGE ( 'NONE', *, *, #5069, .T. ) ;
#4227 = DIRECTION ( 'NONE',  ( 0.000000000000000000, 1.000000000000000000, -0.000000000000000000 ) ) ;
#4228 = AXIS2_PLACEMENT_3D ( 'NONE', #18067, #14515, #2187 ) ;
#4229 = FACE_OUTER_BOUND ( 'NONE', #3704, .T. ) ;
#4230 = FACE_OUTER_BOUND ( 'NONE', #22663, .T. ) ;
#4231 = ORIENTED_EDGE ( 'NONE', *, *, #13180, .T. ) ;
#4232 = ORIENTED_EDGE ( 'NONE', *, *, #2400, .T. ) ;
#4233 = DIRECTION ( 'NONE',  ( 0.4397038457472424167, 0.000000000000000000, 0.8981428216242032248 ) ) ;
#4234 = EDGE_LOOP ( 'NONE', ( #5445, #11256, #17197, #20029 ) ) ;
#4235 = UNCERTAINTY_MEASURE_WITH_UNIT (LENGTH_MEASURE( 1.000000000000000082E-05 ), #18564, 'distance_accuracy_value', 'NONE');
#4236 = CARTESIAN_POINT ( 'NONE',  ( 40.92823665025488822, 108.1171873888033872, 71.55742502417508888 ) ) ;
#4237 = CARTESIAN_POINT ( 'NONE',  ( -89.75533239802831531, 88.06778622492817021, 50.74386735540385018 ) ) ;
#4238 = CARTESIAN_POINT ( 'NONE',  ( 30.95226243471581995, -4.590072317936261470, -0.3747571711140706974 ) ) ;
#4239 = CIRCLE ( 'NONE', #21836, 10.99999999999999289 ) ;
#4241 = ORIENTED_EDGE ( 'NONE', *, *, #18050, .T. ) ;
#4240 = ORIENTED_EDGE ( 'NONE', *, *, #9720, .F. ) ;
#4242 = EDGE_CURVE ( 'NONE', #14514, #9599, #6234, .T. ) ;
#4243 = CARTESIAN_POINT ( 'NONE',  ( -49.94283482827944454, 112.2298613550336057, -43.54035151778127499 ) ) ;
#4244 = ORIENTED_EDGE ( 'NONE', *, *, #9205, .T. ) ;
#4245 = CARTESIAN_POINT ( 'NONE',  ( 3.943435745640934798, 166.6820924781355302, 305.0961849656022764 ) ) ;
#4246 = CARTESIAN_POINT ( 'NONE',  ( -64.99457118636308905, 169.9999999999999716, 0.8400692238016759239 ) ) ;
#4247 = DIRECTION ( 'NONE',  ( 0.000000000000000000, 0.000000000000000000, 1.000000000000000000 ) ) ;
#4248 = DIRECTION ( 'NONE',  ( -0.8789675987075231678, -8.853465811791729457E-23, 0.4768814951561137772 ) ) ;
#4250 = DIRECTION ( 'NONE',  ( -0.01292394549866741384, -0.005513023399720269613, -0.9999012842304692006 ) ) ;
#4249 =( REPRESENTATION_RELATIONSHIP ('NONE','NONE', #11808, #19567 ) REPRESENTATION_RELATIONSHIP_WITH_TRANSFORMATION ( #1157 )SHAPE_REPRESENTATION_RELATIONSHIP( ) );
#4251 = ORIENTED_EDGE ( 'NONE', *, *, #5482, .F. ) ;
#4252 = FACE_OUTER_BOUND ( 'NONE', #5112, .T. ) ;
#4253 = EDGE_LOOP ( 'NONE', ( #4264, #13895, #21323, #19303 ) ) ;
#4254 = FACE_OUTER_BOUND ( 'NONE', #16883, .T. ) ;
#4255 = CARTESIAN_POINT ( 'NONE',  ( -51.82774057240565213, 118.9447701193097942, 172.1955447453271404 ) ) ;
#4256 = CARTESIAN_POINT ( 'NONE',  ( -7.157118525848868984, 144.2648164810658216, 276.0058078322479673 ) ) ;
#4257 = DIRECTION ( 'NONE',  ( -1.000000000000000000, 0.000000000000000000, 2.449293598294706414E-16 ) ) ;
#4258 = FACE_OUTER_BOUND ( 'NONE', #14598, .T. ) ;
#4259 =( LENGTH_UNIT ( ) NAMED_UNIT ( * ) SI_UNIT ( .MILLI., .METRE. ) );
#4260 = CARTESIAN_POINT ( 'NONE',  ( -51.73689940103877660, 111.5659474609696105, -46.65855322351870171 ) ) ;
#4261 = VERTEX_POINT ( 'NONE', #5891 ) ;
#4262 = EDGE_CURVE ( 'NONE', #591, #10951, #13537, .T. ) ;
#4263 = CARTESIAN_POINT ( 'NONE',  ( 12.83416875720839911, 190.4899810681968972, 307.8495766059611469 ) ) ;
#4264 = ORIENTED_EDGE ( 'NONE', *, *, #5813, .F. ) ;
#4265 = EDGE_LOOP ( 'NONE', ( #6241, #9467, #18304, #5417 ) ) ;
#4266 = CARTESIAN_POINT ( 'NONE',  ( -84.60707546407849122, 75.02634323965497742, -1.164978116754957771 ) ) ;
#4267 = CARTESIAN_POINT ( 'NONE',  ( -90.15346953873444136, 88.07696337361356598, 53.07426884559318125 ) ) ;
#4268 =( BOUNDED_CURVE ( )  B_SPLINE_CURVE ( 3, ( #21207, #9263, #9024, #14578 ),
 .UNSPECIFIED., .F., .T. ) 
 B_SPLINE_CURVE_WITH_KNOTS ( ( 4, 4 ),
 ( 3.141592653589793116, 4.712388980384689674 ),
 .UNSPECIFIED. ) 
 CURVE ( )  GEOMETRIC_REPRESENTATION_ITEM ( )  RATIONAL_B_SPLINE_CURVE ( ( 1.000000000000000000, 0.8047378541243649375, 0.8047378541243649375, 1.000000000000000000 ) ) 
 REPRESENTATION_ITEM ( '' )  );
#4269 = EDGE_LOOP ( 'NONE', ( #231, #6753, #21787, #6223 ) ) ;
#4270 = ADVANCED_FACE ( 'NONE', ( #18534 ), #7854, .T. ) ;
#4271 = DIRECTION ( 'NONE',  ( 0.01292394549866738261, 0.005513023399722618428, 0.9999012842304692006 ) ) ;
#4272 = EDGE_CURVE ( 'NONE', #20174, #17225, #9803, .T. ) ;
#4273 = CARTESIAN_POINT ( 'NONE',  ( -37.52478479851671977, 92.78536193177781399, -82.71535724525422495 ) ) ;
#4274 = CARTESIAN_POINT ( 'NONE',  ( 70.91392079944854743, 72.00000000000000000, 84.09052168258639881 ) ) ;
#4275 = EDGE_CURVE ( 'NONE', #10365, #20395, #20111, .T. ) ;
#4276 = ORIENTED_EDGE ( 'NONE', *, *, #5816, .T. ) ;
#4277 = AXIS2_PLACEMENT_3D ( 'NONE', #2540, #20330, #4804 ) ;
#4278 = CARTESIAN_POINT ( 'NONE',  ( 13.80509744631564750, 155.5569384583423300, 100.8921482990249956 ) ) ;
#4279 = CARTESIAN_POINT ( 'NONE',  ( 19.65679901206711477, 183.0231349956771112, 316.5272444403498184 ) ) ;
#4280 = CARTESIAN_POINT ( 'NONE',  ( -5.156377330703261208, 81.99999999999998579, -99.58697729741760440 ) ) ;
#4281 = LINE ( 'NONE', #13158, #6974 ) ;
#4282 = ORIENTED_EDGE ( 'NONE', *, *, #12026, .T. ) ;
#4283 = EDGE_CURVE ( 'NONE', #7668, #10785, #9696, .T. ) ;
#4284 = DIRECTION ( 'NONE',  ( 0.01292394549866737220, 0.005513023399721000799, 0.9999012842304692006 ) ) ;
#4285 = CARTESIAN_POINT ( 'NONE',  ( -45.07718948873534970, 165.9786531560170033, 257.2288776738097908 ) ) ;
#4286 = EDGE_CURVE ( 'NONE', #1373, #10917, #15948, .T. ) ;
#4287 = ORIENTED_EDGE ( 'NONE', *, *, #12481, .T. ) ;
#4288 = LINE ( 'NONE', #2705, #21209 ) ;
#4289 = EDGE_LOOP ( 'NONE', ( #4240, #11007 ) ) ;
#4290 = AXIS2_PLACEMENT_3D ( 'NONE', #13494, #3361, #6802 ) ;
#4291 = CARTESIAN_POINT ( 'NONE',  ( 42.03270152299423756, 106.9589643049704648, 70.53184856292322991 ) ) ;
#4292 = EDGE_CURVE ( 'NONE', #16712, #4358, #14653, .T. ) ;
#4293 = CARTESIAN_POINT ( 'NONE',  ( -45.96195738621045024, 164.6879759653328961, -74.13402305205957532 ) ) ;
#4294 = CYLINDRICAL_SURFACE ( 'NONE', #13320, 6.500000000000000000 ) ;
#4295 = ADVANCED_FACE ( 'NONE', ( #18963 ), #15223, .F. ) ;
#4296 = DIRECTION ( 'NONE',  ( -0.01292394549866745720, -0.005513023399720816918, -0.9999012842304692006 ) ) ;
#4297 = FACE_OUTER_BOUND ( 'NONE', #14760, .T. ) ;
#4298 = EDGE_CURVE ( 'NONE', #20105, #6614, #21900, .T. ) ;
#4299 = VERTEX_POINT ( 'NONE', #15552 ) ;
#4300 = ADVANCED_FACE ( 'NONE', ( #13709 ), #8394, .T. ) ;
#4301 = DIRECTION ( 'NONE',  ( -1.000000000000000000, -4.050949892096651376E-22, 3.955169525227119189E-16 ) ) ;
#4302 = FACE_OUTER_BOUND ( 'NONE', #712, .T. ) ;
#4303 = CIRCLE ( 'NONE', #17165, 6.499999999999998224 ) ;
#4304 = CARTESIAN_POINT ( 'NONE',  ( 91.14374963600242552, 79.10773180776112667, -28.81380175419844747 ) ) ;
#4305 = CARTESIAN_POINT ( 'NONE',  ( -8.326885050334665195, 185.3762957732174073, 323.2536174830050868 ) ) ;
#4306 = AXIS2_PLACEMENT_3D ( 'NONE', #8694, #13892, #20999 ) ;
#4307 = CARTESIAN_POINT ( 'NONE',  ( -38.21549050681395698, 167.4026153394593734, 273.1339171915171846 ) ) ;
#4308 = VERTEX_POINT ( 'NONE', #8621 ) ;
#4309 = CARTESIAN_POINT ( 'NONE',  ( 48.87608419539191829, 189.4960933113125634, -92.09608064579967390 ) ) ;
#4310 = CYLINDRICAL_SURFACE ( 'NONE', #15803, 2.000000000000001332 ) ;
#4311 = CARTESIAN_POINT ( 'NONE',  ( -12.22164657274376154, 182.3338479205205260, 308.9437607284932028 ) ) ;
#4312 = ADVANCED_FACE ( 'NONE', ( #13589 ), #12441, .T. ) ;
#4313 = ORIENTED_EDGE ( 'NONE', *, *, #19177, .T. ) ;
#4314 = EDGE_CURVE ( 'NONE', #784, #7249, #17383, .T. ) ;
#4315 = AXIS2_PLACEMENT_3D ( 'NONE', #10236, #22267, #1185 ) ;
#4316 = ORIENTED_EDGE ( 'NONE', *, *, #11636, .T. ) ;
#4317 = CYLINDRICAL_SURFACE ( 'NONE', #1118, 7.500000000000002665 ) ;
#4318 = EDGE_CURVE ( 'NONE', #8712, #17192, #11639, .T. ) ;
#4319 = TOROIDAL_SURFACE ( 'NONE', #6530, 17.29295143883736330, 7.000000000000003553 ) ;
#4320 = DIRECTION ( 'NONE',  ( -0.01292414190463832269, 0.000000000000000000, -0.9999164797902017066 ) ) ;
#4321 = CARTESIAN_POINT ( 'NONE',  ( 79.92740525950247843, 54.99999999999999289, -6.133505399301337313 ) ) ;
#4322 = ADVANCED_FACE ( 'NONE', ( #22280 ), #15662, .F. ) ;
#4323 = DIRECTION ( 'NONE',  ( -0.9934404589540162256, -0.1135548637187059617, 0.01346653032743144220 ) ) ;
#4324 = AXIS2_PLACEMENT_3D ( 'NONE', #19787, #16734, #877 ) ;
#4325 = ORIENTED_EDGE ( 'NONE', *, *, #11346, .F. ) ;
#4326 = CARTESIAN_POINT ( 'NONE',  ( 82.08478915011154697, 104.7581306074484502, -73.22697298855671022 ) ) ;
#4327 = ORIENTED_EDGE ( 'NONE', *, *, #17265, .F. ) ;
#4328 = CARTESIAN_POINT ( 'NONE',  ( -15.37386863723000907, 178.0286960282952862, 316.7568799295810891 ) ) ;
#4329 = ORIENTED_EDGE ( 'NONE', *, *, #16427, .F. ) ;
#4330 = CARTESIAN_POINT ( 'NONE',  ( -59.90211866468705892, 114.2828829828135042, 169.9016426734428080 ) ) ;
#4331 = DIRECTION ( 'NONE',  ( -0.01292394549866738782, -0.005513023399720700692, -0.9999012842304693116 ) ) ;
#4332 = DIRECTION ( 'NONE',  ( 0.9934404589540163366, 0.1135548637187057675, -0.01346653032742924257 ) ) ;
#4333 = CARTESIAN_POINT ( 'NONE',  ( -40.55787414469111241, 124.9314917220301737, -42.90317659963240970 ) ) ;
#4334 = ORIENTED_EDGE ( 'NONE', *, *, #20873, .F. ) ;
#4335 = ORIENTED_EDGE ( 'NONE', *, *, #9920, .F. ) ;
#4336 = LINE ( 'NONE', #6079, #21118 ) ;
#4337 = CARTESIAN_POINT ( 'NONE',  ( -8.832654921828126504, 186.0492927733070587, 307.0981779263103135 ) ) ;
#4338 = EDGE_CURVE ( 'NONE', #7424, #7803, #15375, .T. ) ;
#4339 = ADVANCED_FACE ( 'NONE', ( #3008 ), #16932, .T. ) ;
#4340 = ORIENTED_EDGE ( 'NONE', *, *, #9653, .F. ) ;
#4341 = VECTOR ( 'NONE', #17635, 1000.000000000000114 ) ;
#4342 = DIRECTION ( 'NONE',  ( 0.000000000000000000, 0.000000000000000000, -1.000000000000000000 ) ) ;
#4343 = CARTESIAN_POINT ( 'NONE',  ( -89.79597934609442689, 88.02156722422921575, 50.77260141037600505 ) ) ;
#4344 = DIRECTION ( 'NONE',  ( 0.9396136610097762798, -0.3422266106549198272, 0.002667396380607422578 ) ) ;
#4346 = ORIENTED_EDGE ( 'NONE', *, *, #4609, .T. ) ;
#4345 = ORIENTED_EDGE ( 'NONE', *, *, #21673, .F. ) ;
#4347 = DIRECTION ( 'NONE',  ( 0.01292394549866739996, 0.005513023399721131770, 0.9999012842304692006 ) ) ;
#4348 = CARTESIAN_POINT ( 'NONE',  ( -52.68156204427607037, 109.2346208036755968, -43.48843840061612553 ) ) ;
#4349 = B_SPLINE_CURVE_WITH_KNOTS ( 'NONE', 3,
 ( #10496, #14067, #1759, #14291, #15791, #3367, #9084, #10384, #15914, #3587, #265, #21162, #17401, #1656, #159, #21051 ),
 .UNSPECIFIED., .F., .F.,
 ( 4, 2, 2, 2, 2, 2, 2, 4 ),
 ( 0.000000000000000000, 0.0003989366781685740491, 0.0007978733563371480982, 0.001196810034505722256, 0.001595746712674296196, 0.001994683390842870354, 0.002393620069011444512, 0.003191493425348546423 ),
 .UNSPECIFIED. ) ;
#4350 = VERTEX_POINT ( 'NONE', #4712 ) ;
#4351 = FACE_OUTER_BOUND ( 'NONE', #6537, .T. ) ;
#4352 = CARTESIAN_POINT ( 'NONE',  ( -61.06315242452672010, 118.9229714579762742, 168.3606140555295951 ) ) ;
#4353 = DIRECTION ( 'NONE',  ( 0.01292394549866743812, 0.005513023399720639109, 0.9999012842304693116 ) ) ;
#4354 = CARTESIAN_POINT ( 'NONE',  ( 0.000000000000000000, 29.00000000000000711, 0.000000000000000000 ) ) ;
#4355 = CARTESIAN_POINT ( 'NONE',  ( 69.43142427201327394, 92.58578643762697880, -85.31868097644085935 ) ) ;
#4356 = ORIENTED_EDGE ( 'NONE', *, *, #18920, .T. ) ;
#4357 = FACE_BOUND ( 'NONE', #16770, .T. ) ;
#4358 = VERTEX_POINT ( 'NONE', #1417 ) ;
#4359 = CARTESIAN_POINT ( 'NONE',  ( -1.163172771417702478, 95.03750572909316929, -89.99248318111824574 ) ) ;
#4360 = CARTESIAN_POINT ( 'NONE',  ( -91.44886093103750113, 77.80125034018028884, -29.89077835665236194 ) ) ;
#4361 = DIRECTION ( 'NONE',  ( -0.000000000000000000, -1.000000000000000000, -0.000000000000000000 ) ) ;
#4362 = CYLINDRICAL_SURFACE ( 'NONE', #11424, 4.200000000000005507 ) ;
#4363 = AXIS2_PLACEMENT_3D ( 'NONE', #16513, #14681, #21635 ) ;
#4364 = ORIENTED_EDGE ( 'NONE', *, *, #9061, .T. ) ;
#4365 = FACE_OUTER_BOUND ( 'NONE', #12111, .T. ) ;
#4366 = DIRECTION ( 'NONE',  ( 8.881784197001252323E-16, 0.000000000000000000, 1.000000000000000000 ) ) ;
#4367 = CIRCLE ( 'NONE', #17219, 3.399999999999991918 ) ;
#4368 = LINE ( 'NONE', #6557, #2549 ) ;
#4369 = VERTEX_POINT ( 'NONE', #10030 ) ;
#4370 = DIRECTION ( 'NONE',  ( -0.000000000000000000, 0.000000000000000000, 1.000000000000000000 ) ) ;
#4371 = ADVANCED_FACE ( 'NONE', ( #19985 ), #11274, .F. ) ;
#4372 = ORIENTED_EDGE ( 'NONE', *, *, #710, .T. ) ;
#4373 = CARTESIAN_POINT ( 'NONE',  ( 3.462212668836658125, 70.69320546282760631, -91.91755708335757902 ) ) ;
#4374 = CARTESIAN_POINT ( 'NONE',  ( -88.16246648193536828, 88.15220846790596454, 52.99592978592204418 ) ) ;
#4375 = DIRECTION ( 'NONE',  ( 0.9999164797902015955, 8.506845633049208051E-18, -0.01292414190464159611 ) ) ;
#4376 = CIRCLE ( 'NONE', #9152, 1.999999999999997780 ) ;
#4378 = ORIENTED_EDGE ( 'NONE', *, *, #6433, .F. ) ;
#4377 = EDGE_LOOP ( 'NONE', ( #12923, #8087, #3825, #12795 ) ) ;
#4379 = AXIS2_PLACEMENT_3D ( 'NONE', #9944, #4747, #10067 ) ;
#4380 = CIRCLE ( 'NONE', #16168, 2.000000000000001332 ) ;
#4381 = CARTESIAN_POINT ( 'NONE',  ( -63.96886132962884375, 101.1306801061894589, 76.70246874139444060 ) ) ;
#4382 = DIRECTION ( 'NONE',  ( -0.01104128644981280764, -0.5197558313507618655, -0.8542435049623797738 ) ) ;
#4383 = DIRECTION ( 'NONE',  ( -0.01292394549866632963, -0.005513023399716958026, -0.9999012842304692006 ) ) ;
#4384 = CARTESIAN_POINT ( 'NONE',  ( 69.75324274910624922, 70.27959272172267902, 85.05633583411396614 ) ) ;
#4385 = CIRCLE ( 'NONE', #19066, 1.999999999999998224 ) ;
#4386 = ORIENTED_EDGE ( 'NONE', *, *, #8773, .F. ) ;
#4387 = CARTESIAN_POINT ( 'NONE',  ( -41.59559178524079215, 173.5443433241884179, 269.1433480140178744 ) ) ;
#4388 = DIRECTION ( 'NONE',  ( -0.9999164797902017066, -2.001050586450178931E-22, 0.01292414190464131508 ) ) ;
#4389 = CARTESIAN_POINT ( 'NONE',  ( 17.35622542770311938, 184.9967961627334887, 319.5060476712728814 ) ) ;
#4390 = DIRECTION ( 'NONE',  ( -2.025474946048326158E-22, 1.000000000000000000, -1.876735158486679638E-22 ) ) ;
#4391 = FACE_OUTER_BOUND ( 'NONE', #12140, .T. ) ;
#4392 = EDGE_LOOP ( 'NONE', ( #6382, #2016, #18881, #20191 ) ) ;
#4393 = SHAPE_REPRESENTATION_RELATIONSHIP ( 'NONE' , 'NONE' ,  #938, #46 ) ;
#4394 = AXIS2_PLACEMENT_3D ( 'NONE', #15938, #12472, #15815 ) ;
#4395 = AXIS2_PLACEMENT_3D ( 'NONE', #11758, #18751, #13598 ) ;
#4396 = B_SPLINE_CURVE_WITH_KNOTS ( 'NONE', 3,
 ( #13532, #6409, #8128, #3165, #13197, #2838, #15038, #3067, #18472, #15273, #13426, #11810, #18909, #15158 ),
 .UNSPECIFIED., .F., .F.,
 ( 4, 2, 2, 2, 2, 2, 4 ),
 ( 0.000000000000000000, 0.001026194940722953983, 0.001539292411084414169, 0.002052389881445874573, 0.003078584822168784537, 0.003591682292530240170, 0.004104779762891694501 ),
 .UNSPECIFIED. ) ;
#4397 = LINE ( 'NONE', #21617, #22013 ) ;
#4398 = LINE ( 'NONE', #14904, #11420 ) ;
#4399 = ORIENTED_EDGE ( 'NONE', *, *, #16149, .T. ) ;
#4400 = AXIS2_PLACEMENT_3D ( 'NONE', #8633, #5070, #15675 ) ;
#4401 = DIRECTION ( 'NONE',  ( -0.9999164797902015955, -2.045733645417851681E-15, 0.01292414190464156835 ) ) ;
#4402 = ORIENTED_EDGE ( 'NONE', *, *, #13888, .F. ) ;
#4403 = EDGE_CURVE ( 'NONE', #6995, #8963, #6337, .T. ) ;
#4404 = VERTEX_POINT ( 'NONE', #1173 ) ;
#4405 = CARTESIAN_POINT ( 'NONE',  ( -9.841028579513169561, 187.8130746588807938, 321.1594247271215750 ) ) ;
#4406 = CIRCLE ( 'NONE', #12852, 3.099999999999998757 ) ;
#4407 = ORIENTED_EDGE ( 'NONE', *, *, #14925, .T. ) ;
#4408 = ORIENTED_EDGE ( 'NONE', *, *, #14566, .T. ) ;
#4409 = CARTESIAN_POINT ( 'NONE',  ( 75.44114733820232743, 75.02649460866172149, 1.289693752222738299 ) ) ;
#4410 = CIRCLE ( 'NONE', #2227, 25.26969600708473962 ) ;
#4411 = CARTESIAN_POINT ( 'NONE',  ( 75.33668001145856863, 75.08929188680230027, 3.154648652659545860 ) ) ;
#4412 =( REPRESENTATION_RELATIONSHIP ('NONE','NONE', #11808, #14914 ) REPRESENTATION_RELATIONSHIP_WITH_TRANSFORMATION ( #445 )SHAPE_REPRESENTATION_RELATIONSHIP( ) );
#4413 = EDGE_CURVE ( 'NONE', #9954, #10082, #19732, .T. ) ;
#4414 = DIRECTION ( 'NONE',  ( -0.4397038457472493556, 0.000000000000000000, -0.8981428216241997831 ) ) ;
#4415 = CIRCLE ( 'NONE', #14723, 85.00000000000001421 ) ;
#4416 = ORIENTED_EDGE ( 'NONE', *, *, #15558, .T. ) ;
#4417 = DIRECTION ( 'NONE',  ( 0.9868605155706532406, 0.1615729028914177079, -0.0007210123890482034170 ) ) ;
#4418 = CARTESIAN_POINT ( 'NONE',  ( -72.65963751957909267, 87.42236182341126494, 69.77244766351077487 ) ) ;
#4419 = FACE_OUTER_BOUND ( 'NONE', #17597, .T. ) ;
#4420 = EDGE_CURVE ( 'NONE', #4059, #8542, #5805, .T. ) ;
#4421 = CARTESIAN_POINT ( 'NONE',  ( 68.58360120290730322, 71.33040186743643574, -86.00170974875821628 ) ) ;
#4422 = FACE_BOUND ( 'NONE', #352, .T. ) ;
#4423 = CIRCLE ( 'NONE', #20190, 1.999999999999997780 ) ;
#4424 = PLANE ( 'NONE',  #21723 ) ;
#4425 = ORIENTED_EDGE ( 'NONE', *, *, #9921, .F. ) ;
#4426 = DIRECTION ( 'NONE',  ( -7.125109674364536131E-05, 0.9999848031710253382, -0.005512562950849706628 ) ) ;
#4427 = VERTEX_POINT ( 'NONE', #11722 ) ;
#4428 = CARTESIAN_POINT ( 'NONE',  ( 65.93268019054301021, 104.4142135623730638, 71.73965483371370055 ) ) ;
#4429 = CARTESIAN_POINT ( 'NONE',  ( -14.35744025451807104, 179.7190799334499332, 309.4176276921488125 ) ) ;
#4430 = ORIENTED_EDGE ( 'NONE', *, *, #8247, .T. ) ;
#4431 = EDGE_CURVE ( 'NONE', #3218, #10523, #329, .T. ) ;
#4432 = EDGE_LOOP ( 'NONE', ( #7899, #917, #11968, #20969 ) ) ;
#4433 = B_SPLINE_CURVE_WITH_KNOTS ( 'NONE', 3,
 ( #17937, #16562, #13000, #7914, #14839, #19967, #11258, #5622 ),
 .UNSPECIFIED., .F., .F.,
 ( 4, 2, 2, 4 ),
 ( 0.005257893453559862873, 0.006567392922673212161, 0.007876892391786561448, 0.01049589133001325308 ),
 .UNSPECIFIED. ) ;
#4434 = VECTOR ( 'NONE', #1685, 1000.000000000000114 ) ;
#4435 = EDGE_CURVE ( 'NONE', #10785, #19030, #5765, .T. ) ;
#4436 = CIRCLE ( 'NONE', #20205, 4.000000000000006217 ) ;
#4437 = ADVANCED_FACE ( 'NONE', ( #19664, #19339 ), #12696, .T. ) ;
#4438 = CARTESIAN_POINT ( 'NONE',  ( 161.9999999999998579, 20.00000000000000000, 10.00000000000220091 ) ) ;
#4439 = CIRCLE ( 'NONE', #10323, 0.3999999999999989120 ) ;
#4440 = EDGE_CURVE ( 'NONE', #18473, #444, #9101, .T. ) ;
#4441 = DIRECTION ( 'NONE',  ( 0.01292394549866738608, 0.005513023399720699824, 0.9999012842304692006 ) ) ;
#4442 = DIRECTION ( 'NONE',  ( 7.125109674403837105E-05, -0.9999848031710252272, 0.005512562950847867821 ) ) ;
#4443 = VERTEX_POINT ( 'NONE', #21064 ) ;
#4444 = EDGE_CURVE ( 'NONE', #1243, #4209, #1074, .T. ) ;
#4445 = VERTEX_POINT ( 'NONE', #16271 ) ;
#4446 = PLANE ( 'NONE',  #14227 ) ;
#4447 = B_SPLINE_CURVE_WITH_KNOTS ( 'NONE', 3,
 ( #2777, #2876, #949, #20548, #21920, #11851 ),
 .UNSPECIFIED., .F., .F.,
 ( 4, 2, 4 ),
 ( 2.403703357979454770E-17, 0.0009937831915592853973, 0.001987566383118546508 ),
 .UNSPECIFIED. ) ;
#4448 = AXIS2_PLACEMENT_3D ( 'NONE', #9926, #20713, #4963 ) ;
#4449 = EDGE_CURVE ( 'NONE', #19436, #15988, #10851, .T. ) ;
#4450 = CARTESIAN_POINT ( 'NONE',  ( -8.747090466623152594, 185.2634439126724999, 305.1792882774458917 ) ) ;
#4451 = ORIENTED_EDGE ( 'NONE', *, *, #12740, .F. ) ;
#4452 = EDGE_LOOP ( 'NONE', ( #10417, #6060, #1418, #22286 ) ) ;
#4453 = CARTESIAN_POINT ( 'NONE',  ( -60.77640960548244919, 114.5357201574170176, 168.7587714564542694 ) ) ;
#4454 = CARTESIAN_POINT ( 'NONE',  ( -38.71138566794451918, 96.73515328252067036, 84.40350015143866358 ) ) ;
#4455 = DIRECTION ( 'NONE',  ( 0.01292394549867042185, 0.005513023399718316314, 0.9999012842304693116 ) ) ;
#4456 = VERTEX_POINT ( 'NONE', #17763 ) ;
#4457 = CARTESIAN_POINT ( 'NONE',  ( 65.34146690339817098, 126.1473081376433498, 25.99859803869739139 ) ) ;
#4458 = AXIS2_PLACEMENT_3D ( 'NONE', #13144, #13378, #16719 ) ;
#4459 = CARTESIAN_POINT ( 'NONE',  ( -26.20953091143350377, 324.3346178683207768, 319.1363590876133571 ) ) ;
#4460 = EDGE_CURVE ( 'NONE', #7165, #9573, #10426, .T. ) ;
#4461 = VERTEX_POINT ( 'NONE', #173 ) ;
#4462 = AXIS2_PLACEMENT_3D ( 'NONE', #1143, #1266, #4455 ) ;
#4463 = AXIS2_PLACEMENT_3D ( 'NONE', #16763, #10084, #11580 ) ;
#4464 = AXIS2_PLACEMENT_3D ( 'NONE', #576, #12752, #3783 ) ;
#4465 = CARTESIAN_POINT ( 'NONE',  ( -88.17195568186734533, 88.85982347399621517, 52.11040125407321000 ) ) ;
#4466 = APPLICATION_PROTOCOL_DEFINITION ( 'draft international standard', 'automotive_design', 1998, #1483 ) ;
#4467 = ORIENTED_EDGE ( 'NONE', *, *, #19647, .F. ) ;
#4468 = CARTESIAN_POINT ( 'NONE',  ( -49.26081312276134838, 111.2483156817622927, -43.54375498084313278 ) ) ;
#4469 = CARTESIAN_POINT ( 'NONE',  ( 13.04687021101641342, 190.3009381008880609, 320.8498765639175190 ) ) ;
#4470 = DIRECTION ( 'NONE',  ( -0.01292394549866727679, -0.005513023399720742325, -0.9999012842304692006 ) ) ;
#4471 = CARTESIAN_POINT ( 'NONE',  ( 161.9999999999998863, 20.00000000000000000, 8.000000000002200906 ) ) ;
#4472 = DIRECTION ( 'NONE',  ( -0.9999164797902015955, -2.457859219970326020E-15, 0.01292414190464043211 ) ) ;
#4473 = CARTESIAN_POINT ( 'NONE',  ( -48.67250884018650225, 109.5699351474431467, -43.54210507929712293 ) ) ;
#4474 = CARTESIAN_POINT ( 'NONE',  ( -59.98899403950397158, 118.2576901802692504, 47.66399645013669328 ) ) ;
#4475 = VERTEX_POINT ( 'NONE', #7169 ) ;
#4476 = EDGE_CURVE ( 'NONE', #4193, #21164, #14557, .T. ) ;
#4477 = DIRECTION ( 'NONE',  ( -0.9250486434174662875, -0.3795887553195633202, 0.01404934683357507604 ) ) ;
#4478 = ORIENTED_EDGE ( 'NONE', *, *, #15979, .T. ) ;
#4479 = CARTESIAN_POINT ( 'NONE',  ( -72.65712060336477407, 87.67824255507785836, 70.07990617929104360 ) ) ;
#4480 = CARTESIAN_POINT ( 'NONE',  ( -75.30975508861040169, 94.90914755154933857, 80.17755788556743823 ) ) ;
#4481 = DIRECTION ( 'NONE',  ( 0.01292394549866727679, 0.005513023399720742325, 0.9999012842304692006 ) ) ;
#4482 = DIRECTION ( 'NONE',  ( 0.000000000000000000, 1.000000000000000000, -0.000000000000000000 ) ) ;
#4483 = VECTOR ( 'NONE', #4639, 1000.000000000000227 ) ;
#4484 = AXIS2_PLACEMENT_3D ( 'NONE', #13520, #777, #16753 ) ;
#4485 = ORIENTED_EDGE ( 'NONE', *, *, #1223, .T. ) ;
#4486 = DIRECTION ( 'NONE',  ( 7.125109674160325297E-05, -0.9999848031710252272, 0.005512562950849327591 ) ) ;
#4487 = CARTESIAN_POINT ( 'NONE',  ( -51.64677849790292186, 114.5530515816765416, 171.7847092408061656 ) ) ;
#4488 = VERTEX_POINT ( 'NONE', #12463 ) ;
#4489 = FACE_BOUND ( 'NONE', #21574, .T. ) ;
#4490 = ADVANCED_FACE ( 'NONE', ( #19448 ), #7662, .T. ) ;
#4491 = CONICAL_SURFACE ( 'NONE', #5953, 4.999999999999990230, 1.047197551196595855 ) ;
#4492 = DIRECTION ( 'NONE',  ( 0.000000000000000000, 0.000000000000000000, 1.000000000000000000 ) ) ;
#4493 = ORIENTED_EDGE ( 'NONE', *, *, #1363, .T. ) ;
#4494 = CARTESIAN_POINT ( 'NONE',  ( -1.702894481557716944, 157.8934747572109814, 324.0533643900782295 ) ) ;
#4495 = CARTESIAN_POINT ( 'NONE',  ( -90.17314623510533522, 87.05539508966613482, 51.36443554363990671 ) ) ;
#4497 = LINE ( 'NONE', #9798, #2352 ) ;
#4496 = AXIS2_PLACEMENT_3D ( 'NONE', #14594, #12742, #5819 ) ;
#4498 = ORIENTED_EDGE ( 'NONE', *, *, #18557, .F. ) ;
#4499 = CIRCLE ( 'NONE', #7443, 101.0000000000000000 ) ;
#4500 = DIRECTION ( 'NONE',  ( 7.125109674161246868E-05, -0.9999848031710252272, 0.005512562950850154186 ) ) ;
#4501 = DIRECTION ( 'NONE',  ( 7.125109674403277385E-05, -0.9999848031710253382, 0.005512562950848281552 ) ) ;
#4502 = DIRECTION ( 'NONE',  ( 7.125109674161246868E-05, -0.9999848031710253382, 0.005512562950850155054 ) ) ;
#4503 = DIRECTION ( 'NONE',  ( 0.01292394549866738608, 0.005513023399720699824, 0.9999012842304692006 ) ) ;
#4504 = CARTESIAN_POINT ( 'NONE',  ( 70.91392079944856164, 71.82437938702648239, 84.09052168258639881 ) ) ;
#4505 = ADVANCED_FACE ( 'NONE', ( #21279 ), #5546, .F. ) ;
#4506 = VERTEX_POINT ( 'NONE', #392 ) ;
#4507 = EDGE_CURVE ( 'NONE', #12879, #1725, #7386, .T. ) ;
#4508 = CARTESIAN_POINT ( 'NONE',  ( -57.55221044392004615, 114.6951352185433421, 172.9675203174990088 ) ) ;
#4509 = DIRECTION ( 'NONE',  ( -0.9999164797902015955, 8.863511990578706951E-16, 0.01292414190464158050 ) ) ;
#4510 = CARTESIAN_POINT ( 'NONE',  ( 19.89301572175062560, 183.5588582068999131, 313.6515632266070384 ) ) ;
#4511 = DIRECTION ( 'NONE',  ( 0.01292394549866738608, 0.005513023399720698957, 0.9999012842304692006 ) ) ;
#4512 = DIRECTION ( 'NONE',  ( -1.000000000000000000, 0.000000000000000000, -1.362186893977296347E-14 ) ) ;
#4513 = EDGE_LOOP ( 'NONE', ( #15106, #1039, #20699 ) ) ;
#4514 = CARTESIAN_POINT ( 'NONE',  ( 0.000000000000000000, 0.000000000000000000, 0.000000000000000000 ) ) ;
#4515 = AXIS2_PLACEMENT_3D ( 'NONE', #3150, #12121, #8319 ) ;
#4516 = CIRCLE ( 'NONE', #1612, 2.000000000000001332 ) ;
#4517 = DIRECTION ( 'NONE',  ( -0.9999164797902017066, -2.001050586450178931E-22, 0.01292414190464131508 ) ) ;
#4518 = DIRECTION ( 'NONE',  ( -0.01292414190464131335, 0.000000000000000000, -0.9999164797902015955 ) ) ;
#4519 = VERTEX_POINT ( 'NONE', #20108 ) ;
#4520 = DIRECTION ( 'NONE',  ( 0.9232306267972774094, 0.000000000000000000, -0.3842462878721227826 ) ) ;
#4521 = ORIENTED_EDGE ( 'NONE', *, *, #7164, .F. ) ;
#4522 = PRODUCT_RELATED_PRODUCT_CATEGORY ( 'part', '', ( #8844 ) ) ;
#4523 = DIRECTION ( 'NONE',  ( 0.1136178953597579422, -0.9935164314186355483, 0.004009283626633659663 ) ) ;
#4524 = ORIENTED_EDGE ( 'NONE', *, *, #15793, .F. ) ;
#4525 = CIRCLE ( 'NONE', #21716, 2.000000000000001332 ) ;
#4526 = CIRCLE ( 'NONE', #21026, 126.0000000000000000 ) ;
#4527 = ORIENTED_EDGE ( 'NONE', *, *, #13731, .T. ) ;
#4528 = DIRECTION ( 'NONE',  ( 2.025474946048326158E-22, -1.000000000000000000, 1.876735158486679638E-22 ) ) ;
#4529 = DIRECTION ( 'NONE',  ( 2.025474946048326158E-22, -1.000000000000000000, 1.876735158486679638E-22 ) ) ;
#4530 = DIRECTION ( 'NONE',  ( -0.9999164797902017066, -2.775557561562891351E-15, 0.01292414190464108437 ) ) ;
#4531 = VECTOR ( 'NONE', #12580, 1000.000000000000000 ) ;
#4532 = CARTESIAN_POINT ( 'NONE',  ( -107.9412751340845773, 77.72595396897818887, -21.65777188997713765 ) ) ;
#4533 = DIRECTION ( 'NONE',  ( -0.000000000000000000, -1.000000000000000000, -0.000000000000000000 ) ) ;
#4534 = CARTESIAN_POINT ( 'NONE',  ( 13.04156242531480991, 188.9519362114520220, 275.7250501837552861 ) ) ;
#4535 = EDGE_LOOP ( 'NONE', ( #4386, #11606, #21208 ) ) ;
#4536 = LINE ( 'NONE', #20611, #17608 ) ;
#4537 = DIRECTION ( 'NONE',  ( -0.01292394549866740169, -0.005513023399721270548, -0.9999012842304692006 ) ) ;
#4538 = DIRECTION ( 'NONE',  ( -0.9999164797902015955, 0.000000000000000000, 0.01292414190464162733 ) ) ;
#4539 = DIRECTION ( 'NONE',  ( -0.9999164797902015955, -2.001050586450178695E-22, 0.01292414190464131335 ) ) ;
#4540 = CARTESIAN_POINT ( 'NONE',  ( 89.76942472236373760, 79.35227432041557449, -29.58847612530787075 ) ) ;
#4541 = CARTESIAN_POINT ( 'NONE',  ( 93.18852247616533191, 70.03011042807717956, 58.44685241948164389 ) ) ;
#4542 = AXIS2_PLACEMENT_3D ( 'NONE', #6910, #1648, #24 ) ;
#4543 = CARTESIAN_POINT ( 'NONE',  ( 49.06618554817806910, 189.4933803444196201, -92.59067283796298398 ) ) ;
#4544 = EDGE_LOOP ( 'NONE', ( #14404, #10765, #20683, #727 ) ) ;
#4545 = DIRECTION ( 'NONE',  ( 0.009760756503427210282, -0.9999378516499566327, 0.005387065077606872227 ) ) ;
#4546 = CARTESIAN_POINT ( 'NONE',  ( -10.58768000256260855, 183.8591665011366842, 305.6983654296078043 ) ) ;
#4547 = ORIENTED_EDGE ( 'NONE', *, *, #14878, .F. ) ;
#4548 = VECTOR ( 'NONE', #1170, 1000.000000000000114 ) ;
#4549 = ORIENTED_EDGE ( 'NONE', *, *, #12097, .F. ) ;
#4550 = CIRCLE ( 'NONE', #12259, 5.099999999999992539 ) ;
#4551 = APPLICATION_CONTEXT ( 'automotive_design' ) ;
#4552 = CARTESIAN_POINT ( 'NONE',  ( 51.07319921393754214, 94.45452722259994971, 82.70828171889884572 ) ) ;
#4553 = AXIS2_PLACEMENT_3D ( 'NONE', #17931, #19623, #12753 ) ;
#4554 = CARTESIAN_POINT ( 'NONE',  ( 0.3024632767450905479, 327.3415402339139746, 312.9481704872475234 ) ) ;
#4555 = DIRECTION ( 'NONE',  ( 0.8646325210002208106, -0.1131488163178875073, 0.4894976496313986902 ) ) ;
#4556 = FACE_OUTER_BOUND ( 'NONE', #11973, .T. ) ;
#4557 = EDGE_CURVE ( 'NONE', #5284, #10079, #19891, .T. ) ;
#4558 = ORIENTED_EDGE ( 'NONE', *, *, #8262, .T. ) ;
#4559 = VECTOR ( 'NONE', #21959, 1000.000000000000000 ) ;
#4560 = ADVANCED_FACE ( 'NONE', ( #13226 ), #16454, .T. ) ;
#4561 = CARTESIAN_POINT ( 'NONE',  ( -15.56327362081419885, 177.7277181364938485, 314.9118054635637236 ) ) ;
#4562 = ORIENTED_EDGE ( 'NONE', *, *, #12066, .F. ) ;
#4563 = DIRECTION ( 'NONE',  ( 7.125109674160258889E-05, -0.9999848031710253382, 0.005512562950849898315 ) ) ;
#4564 = CARTESIAN_POINT ( 'NONE',  ( -38.13965839584966488, 96.20077325653890910, 84.87509721996781309 ) ) ;
#4565 = CARTESIAN_POINT ( 'NONE',  ( 67.43998885458336190, 192.1904093341285886, 33.60813087397579579 ) ) ;
#4566 = ORIENTED_EDGE ( 'NONE', *, *, #8797, .F. ) ;
#4567 = LINE ( 'NONE', #18590, #15826 ) ;
#4568 = DIRECTION ( 'NONE',  ( 1.372099599554306628E-14, -0.000000000000000000, -1.000000000000000000 ) ) ;
#4569 = CARTESIAN_POINT ( 'NONE',  ( 21.07318851263119441, 147.3427684080706115, 276.4785941130655829 ) ) ;
#4570 = VECTOR ( 'NONE', #264, 999.9999999999998863 ) ;
#4571 = CARTESIAN_POINT ( 'NONE',  ( -56.88982296092829927, 126.2575686056374735, 47.57983110662551951 ) ) ;
#4572 = ADVANCED_FACE ( 'NONE', ( #21688 ), #19857, .T. ) ;
#4573 = ORIENTED_EDGE ( 'NONE', *, *, #1098, .F. ) ;
#4574 = DIRECTION ( 'NONE',  ( -0.9999164797902015955, -6.965998958219364448E-18, 0.01292414190464157182 ) ) ;
#4575 = CARTESIAN_POINT ( 'NONE',  ( -44.20351303877662019, 168.2403975157799607, 277.2070894419563274 ) ) ;
#4576 = ADVANCED_FACE ( 'NONE', ( #9771 ), #717, .F. ) ;
#4577 = SHAPE_DEFINITION_REPRESENTATION ( #12158, #2270 ) ;
#4579 = ORIENTED_EDGE ( 'NONE', *, *, #3039, .T. ) ;
#4578 = ORIENTED_EDGE ( 'NONE', *, *, #12470, .T. ) ;
#4580 = LINE ( 'NONE', #13012, #9122 ) ;
#4581 = CARTESIAN_POINT ( 'NONE',  ( -50.68129816702384005, 109.3835034331725780, -45.87488247214934489 ) ) ;
#4582 = EDGE_LOOP ( 'NONE', ( #15004, #4855, #2910 ) ) ;
#4583 = DIRECTION ( 'NONE',  ( -0.9934404589540164476, -0.1135548637187044213, 0.01346653032743048289 ) ) ;
#4584 = DIRECTION ( 'NONE',  ( 0.000000000000000000, -1.000000000000000000, 0.000000000000000000 ) ) ;
#4585 = AXIS2_PLACEMENT_3D ( 'NONE', #14722, #808, #2521 ) ;
#4586 = CARTESIAN_POINT ( 'NONE',  ( 9.142505149400548703, 81.99999999999998579, -88.65345271381772818 ) ) ;
#4587 = B_SPLINE_SURFACE_WITH_KNOTS ( 'NONE', 3, 1, ( 
 ( #3875, #19375 ),
 ( #17562, #1813 ),
 ( #7091, #14123 ),
 ( #1934, #210 ),
 ( #7206, #14237 ),
 ( #21212, #5467 ),
 ( #12504, #19490 ),
 ( #16081, #322 ),
 ( #7313, #21325 ),
 ( #5593, #12628 ),
 ( #15763, #14040 ),
 ( #5158, #10467 ),
 ( #16106, #6887 ),
 ( #17483, #22596 ),
 ( #6, #19182 ),
 ( #21022, #13910 ),
 ( #350, #21236 ),
 ( #1734, #19065 ),
 ( #128, #12200 ),
 ( #5501, #239 ),
 ( #12532, #20901 ),
 ( #8955, #7233 ),
 ( #12319, #16000 ),
 ( #7128, #7009 ),
 ( #5275, #17719 ),
 ( #8610, #7342 ),
 ( #3669, #3454 ),
 ( #8711, #15652 ),
 ( #19296, #1965 ),
 ( #14263, #3560 ),
 ( #10572, #17594 ),
 ( #3336, #19526 ),
 ( #3793, #14156 ),
 ( #10815, #21135 ),
 ( #10358, #1840 ),
 ( #8838, #5381 ) ),
 .UNSPECIFIED., .F., .F., .F.,
 ( 4, 3, 2, 2, 2, 2, 2, 2, 2, 2, 2, 2, 2, 2, 2, 3, 4 ),
 ( 2, 2 ),
 ( -0.01000000000000000021, 0.000000000000000000, 0.1249999999999998335, 0.1874999999999999167, 0.2500000000000000000, 0.3125000000000000555, 0.3750000000000001665, 0.4375000000000002220, 0.5000000000000003331, 0.5625000000000003331, 0.6250000000000003331, 0.6875000000000004441, 0.7500000000000004441, 0.8125000000000004441, 0.8750000000000004441, 1.000000000000000000, 1.010000000000000009 ),
 ( 0.000000000000000000, 1.000000000000000000 ),
 .UNSPECIFIED. ) ;
#4588 = CYLINDRICAL_SURFACE ( 'NONE', #21872, 1.999999999999997780 ) ;
#4589 = DIRECTION ( 'NONE',  ( 7.125109674161246868E-05, -0.9999848031710253382, 0.005512562950850155054 ) ) ;
#4590 = ORIENTED_EDGE ( 'NONE', *, *, #17530, .F. ) ;
#4591 = EDGE_CURVE ( 'NONE', #14146, #15447, #4580, .T. ) ;
#4592 = DIRECTION ( 'NONE',  ( -5.440186201345785633E-18, -1.000000000000000000, -1.334940939666367878E-17 ) ) ;
#4593 = ORIENTED_EDGE ( 'NONE', *, *, #14843, .T. ) ;
#4594 = CYLINDRICAL_SURFACE ( 'NONE', #12526, 5.099999999999994316 ) ;
#4595 = CARTESIAN_POINT ( 'NONE',  ( -77.73934989822751618, 90.41888789451962793, 77.89547054214936850 ) ) ;
#4596 = LINE ( 'NONE', #21014, #655 ) ;
#4597 = CARTESIAN_POINT ( 'NONE',  ( -158.3970384574724335, 20.00000000000000000, -62.74304228515459414 ) ) ;
#4598 = ADVANCED_FACE ( 'NONE', ( #1034 ), #16501, .F. ) ;
#4599 = PLANE ( 'NONE',  #3769 ) ;
#4600 = DIRECTION ( 'NONE',  ( -5.440186201345739411E-18, -1.000000000000000000, -1.334940939666364181E-17 ) ) ;
#4601 = ORIENTED_EDGE ( 'NONE', *, *, #10128, .T. ) ;
#4602 = DIRECTION ( 'NONE',  ( -1.396592535537253658E-14, 0.000000000000000000, -1.000000000000000000 ) ) ;
#4603 = DIRECTION ( 'NONE',  ( -0.01292394549866741384, -0.005513023399720269613, -0.9999012842304692006 ) ) ;
#4604 = EDGE_LOOP ( 'NONE', ( #2206, #1422, #13239, #5708 ) ) ;
#4605 = TOROIDAL_SURFACE ( 'NONE', #1327, 93.00000000000000000, 2.000000000000000000 ) ;
#4606 = ORIENTED_EDGE ( 'NONE', *, *, #4162, .F. ) ;
#4607 = DIRECTION ( 'NONE',  ( 0.01111468050521610164, -0.5103046645782707280, 0.8599218645824314722 ) ) ;
#4608 = CARTESIAN_POINT ( 'NONE',  ( -88.16421018802580534, 88.33740264743815374, 52.84970504259129598 ) ) ;
#4609 = EDGE_CURVE ( 'NONE', #18970, #7858, #18502, .T. ) ;
#4611 = ORIENTED_EDGE ( 'NONE', *, *, #1301, .F. ) ;
#4610 = VERTEX_POINT ( 'NONE', #9534 ) ;
#4612 = CARTESIAN_POINT ( 'NONE',  ( 59.61913581103840443, 126.9053488551049611, 163.5819556846717546 ) ) ;
#4613 = FACE_OUTER_BOUND ( 'NONE', #13813, .T. ) ;
#4614 = CARTESIAN_POINT ( 'NONE',  ( 11.12049972950270416, 140.4778767860208859, 86.62632701596898244 ) ) ;
#4615 = ORIENTED_EDGE ( 'NONE', *, *, #1551, .T. ) ;
#4616 = ORIENTED_EDGE ( 'NONE', *, *, #6425, .F. ) ;
#4617 = DIRECTION ( 'NONE',  ( -0.01104128644981183967, -0.5197558313507629757, -0.8542435049623791077 ) ) ;
#4618 = CARTESIAN_POINT ( 'NONE',  ( -88.95538863342423497, 79.66477516473727860, 30.55627054544664034 ) ) ;
#4619 = CARTESIAN_POINT ( 'NONE',  ( 3.316611465012865967, 166.4147053302257007, 256.5999727791399323 ) ) ;
#4620 = EDGE_CURVE ( 'NONE', #848, #14385, #16569, .T. ) ;
#4621 = ORIENTED_EDGE ( 'NONE', *, *, #10061, .F. ) ;
#4622 = EDGE_LOOP ( 'NONE', ( #17955, #1764, #19535, #22327, #11317 ) ) ;
#4623 = CARTESIAN_POINT ( 'NONE',  ( -88.82263333796721838, 169.9999999999999716, 1.148052203164671159 ) ) ;
#4624 = CARTESIAN_POINT ( 'NONE',  ( -56.14669609475481593, 126.5745674511214673, 105.0741549498773679 ) ) ;
#4625 = CARTESIAN_POINT ( 'NONE',  ( 0.000000000000000000, 37.00000000000000711, -78.99999999999998579 ) ) ;
#4626 = CARTESIAN_POINT ( 'NONE',  ( -38.63447605617402303, 163.9374297322429470, 277.1588331099309812 ) ) ;
#4627 = CARTESIAN_POINT ( 'NONE',  ( -6.127092384110496504, 143.9207436052761011, 275.8026882763405183 ) ) ;
#4628 = ORIENTED_EDGE ( 'NONE', *, *, #1917, .F. ) ;
#4629 =( LENGTH_UNIT ( ) NAMED_UNIT ( * ) SI_UNIT ( .MILLI., .METRE. ) );
#4630 = CARTESIAN_POINT ( 'NONE',  ( 158.3970384574715808, 18.00000000000000355, 62.74304228515676130 ) ) ;
#4631 = CARTESIAN_POINT ( 'NONE',  ( -10.47529108877129289, 187.0770174862624629, 321.0793257476343570 ) ) ;
#4632 = VERTEX_POINT ( 'NONE', #12881 ) ;
#4633 = ORIENTED_EDGE ( 'NONE', *, *, #18894, .T. ) ;
#4634 = CARTESIAN_POINT ( 'NONE',  ( -1.163172771417702700, 69.99999999999998579, -89.99248318111824574 ) ) ;
#4635 = ADVANCED_FACE ( 'NONE', ( #6086 ), #16354, .T. ) ;
#4636 = EDGE_CURVE ( 'NONE', #7423, #9056, #6573, .T. ) ;
#4637 = VERTEX_POINT ( 'NONE', #14617 ) ;
#4638 = DIRECTION ( 'NONE',  ( 0.9999164797902015955, 0.000000000000000000, -0.01292414190463754553 ) ) ;
#4639 = DIRECTION ( 'NONE',  ( -0.9726991065672921932, -0.2316562896908778701, 0.01384960395994898341 ) ) ;
#4640 = CARTESIAN_POINT ( 'NONE',  ( 86.06165675176548291, 75.01312404301673098, 0.5177417398328088005 ) ) ;
#4641 = CARTESIAN_POINT ( 'NONE',  ( 163.9999999999998579, 0.000000000000000000, 10.00000000000222933 ) ) ;
#4642 = CARTESIAN_POINT ( 'NONE',  ( 16.06222704467468176, 187.3778571219613127, 276.4007913481239029 ) ) ;
#4643 = FACE_OUTER_BOUND ( 'NONE', #18554, .T. ) ;
#4644 = DIRECTION ( 'NONE',  ( -0.01292394549866737741, -0.005513023399721125699, -0.9999012842304693116 ) ) ;
#4645 = DIRECTION ( 'NONE',  ( -0.5089394657577703818, -0.004781488884709769391, -0.8607890319690654213 ) ) ;
#4646 = CYLINDRICAL_SURFACE ( 'NONE', #16554, 10.99999999999999289 ) ;
#4647 = DIRECTION ( 'NONE',  ( 0.01292394549866733404, 0.005513023399720420534, 0.9999012842304693116 ) ) ;
#4648 = ORIENTED_EDGE ( 'NONE', *, *, #9720, .T. ) ;
#4649 = ORIENTED_EDGE ( 'NONE', *, *, #14599, .F. ) ;
#4650 = CARTESIAN_POINT ( 'NONE',  ( -14.37443239621853408, 105.6999454642524654, 127.3358366182947634 ) ) ;
#4651 = CARTESIAN_POINT ( 'NONE',  ( -8.455960479418571651, 185.4572466408051241, 305.1464658859009660 ) ) ;
#4652 = ORIENTED_EDGE ( 'NONE', *, *, #14489, .T. ) ;
#4653 = CARTESIAN_POINT ( 'NONE',  ( -41.47069032946998846, 166.0668615304125808, 273.1833561390217824 ) ) ;
#4654 = ORIENTED_EDGE ( 'NONE', *, *, #11950, .F. ) ;
#4655 = CARTESIAN_POINT ( 'NONE',  ( 51.64670511766545502, 84.99999999999997158, -27.66980033337678790 ) ) ;
#4656 = CARTESIAN_POINT ( 'NONE',  ( -1.163172771417702700, 81.99999999999998579, -89.99248318111824574 ) ) ;
#4657 = CIRCLE ( 'NONE', #13852, 6.500000000000000000 ) ;
#4658 = CARTESIAN_POINT ( 'NONE',  ( -66.42677970909001317, 189.3893605493459233, -109.9672025422466959 ) ) ;
#4659 = CARTESIAN_POINT ( 'NONE',  ( -1.163172771417702700, 37.00000000000000711, -89.99248318111824574 ) ) ;
#4660 = CARTESIAN_POINT ( 'NONE',  ( -11.71580855312696201, 182.8374334212718395, 306.3219252926489276 ) ) ;
#4661 = ORIENTED_EDGE ( 'NONE', *, *, #20081, .T. ) ;
#4662 = CARTESIAN_POINT ( 'NONE',  ( 16.39634482804422433, 187.9401017119210451, 319.7988598509798521 ) ) ;
#4663 = CYLINDRICAL_SURFACE ( 'NONE', #13750, 96.00000000000000000 ) ;
#4664 = LINE ( 'NONE', #9978, #7034 ) ;
#4665 = ORIENTED_EDGE ( 'NONE', *, *, #14997, .F. ) ;
#4666 = DIRECTION ( 'NONE',  ( 0.000000000000000000, -1.000000000000000000, 0.000000000000000000 ) ) ;
#4667 = CARTESIAN_POINT ( 'NONE',  ( -72.65623182917823897, 87.80665977804258659, 70.23323934248251987 ) ) ;
#4668 = LINE ( 'NONE', #11703, #10657 ) ;
#4669 = ADVANCED_FACE ( 'NONE', ( #8029 ), #21906, .T. ) ;
#4670 = AXIS2_PLACEMENT_3D ( 'NONE', #21347, #17710, #233 ) ;
#4671 = CARTESIAN_POINT ( 'NONE',  ( -27.41563077536688908, 324.1610551366917434, 310.3061288224688496 ) ) ;
#4672 = EDGE_CURVE ( 'NONE', #17969, #724, #1439, .T. ) ;
#4673 = FACE_OUTER_BOUND ( 'NONE', #21738, .T. ) ;
#4674 = DIRECTION ( 'NONE',  ( -0.01292394549866739996, -0.005513023399721131770, -0.9999012842304692006 ) ) ;
#4675 = ITEM_DEFINED_TRANSFORMATION ( 'NONE', 'NONE', #9227,  #6292 ) ;
#4677 = ORIENTED_EDGE ( 'NONE', *, *, #6844, .F. ) ;
#4676 = ORIENTED_EDGE ( 'NONE', *, *, #7112, .T. ) ;
#4678 = CARTESIAN_POINT ( 'NONE',  ( 90.64608739977012419, 77.80075968338644543, -32.24365086765053690 ) ) ;
#4679 = CARTESIAN_POINT ( 'NONE',  ( -40.65822637310711940, 69.99999999999998579, -84.25167897319538213 ) ) ;
#4680 = DIRECTION ( 'NONE',  ( -0.01292394549866727679, -0.005513023399720742325, -0.9999012842304692006 ) ) ;
#4681 = CARTESIAN_POINT ( 'NONE',  ( -55.33804461215960657, 114.2193244133317904, 167.6379947637574617 ) ) ;
#4682 = LINE ( 'NONE', #11717, #10495 ) ;
#4683 = CARTESIAN_POINT ( 'NONE',  ( -10.79665701538697320, 105.7314194667820004, 132.9990107322359449 ) ) ;
#4684 = STYLED_ITEM ( 'NONE', ( #3857 ), #1915 ) ;
#4685 = CARTESIAN_POINT ( 'NONE',  ( 19.43891449096291169, 175.6145212674599065, 111.2097777439524151 ) ) ;
#4686 = EDGE_CURVE ( 'NONE', #5262, #19478, #1802, .T. ) ;
#4687 = ORIENTED_EDGE ( 'NONE', *, *, #18226, .T. ) ;
#4688 = CARTESIAN_POINT ( 'NONE',  ( 35.70966224000307676, 93.64690829573217457, -83.82160924484935549 ) ) ;
#4689 = CARTESIAN_POINT ( 'NONE',  ( 41.19609277020862947, 125.3640259171584290, 247.0300997508393266 ) ) ;
#4690 = ORIENTED_EDGE ( 'NONE', *, *, #18087, .T. ) ;
#4691 = PLANE ( 'NONE',  #5915 ) ;
#4692 = CARTESIAN_POINT ( 'NONE',  ( 0.000000000000000000, 37.00000000000000711, 0.000000000000000000 ) ) ;
#4693 = DIRECTION ( 'NONE',  ( -0.01292394549866743465, -0.005513023399721021615, -0.9999012842304692006 ) ) ;
#4694 = DIRECTION ( 'NONE',  ( -0.01292394549866739822, -0.005513023399721269681, -0.9999012842304692006 ) ) ;
#4695 = ADVANCED_FACE ( 'NONE', ( #18706 ), #8828, .T. ) ;
#4696 = CARTESIAN_POINT ( 'NONE',  ( 58.09925391635511005, 144.7594389791739218, 45.99156051245947907 ) ) ;
#4697 = LINE ( 'NONE', #2783, #15243 ) ;
#4698 = AXIS2_PLACEMENT_3D ( 'NONE', #11868, #13482, #22500 ) ;
#4699 = VERTEX_POINT ( 'NONE', #791 ) ;
#4700 = DIRECTION ( 'NONE',  ( -1.000000000000000000, 0.000000000000000000, 1.396592535537260757E-14 ) ) ;
#4701 = CARTESIAN_POINT ( 'NONE',  ( -34.77142196148174946, 121.3072273804455250, 250.0345615839236757 ) ) ;
#4702 = AXIS2_PLACEMENT_3D ( 'NONE', #17485, #19409, #20686 ) ;
#4703 = ORIENTED_EDGE ( 'NONE', *, *, #7647, .T. ) ;
#4704 = EDGE_CURVE ( 'NONE', #1703, #4037, #12814, .T. ) ;
#4705 = LINE ( 'NONE', #18853, #10957 ) ;
#4706 = CARTESIAN_POINT ( 'NONE',  ( -90.01244464125365141, 88.69783294518954619, 52.52355859850199238 ) ) ;
#4707 = ADVANCED_FACE ( 'NONE', ( #2739 ), #6297, .T. ) ;
#4708 = ADVANCED_FACE ( 'NONE', ( #722 ), #11705, .T. ) ;
#4709 = EDGE_LOOP ( 'NONE', ( #12134, #6691, #10533, #3291 ) ) ;
#4710 = CARTESIAN_POINT ( 'NONE',  ( 52.34460878051607580, 78.91761970611439381, 26.32568957529414178 ) ) ;
#4711 = CARTESIAN_POINT ( 'NONE',  ( -74.32951741256083267, 95.10877321710717069, 82.85879239736101454 ) ) ;
#4712 = CARTESIAN_POINT ( 'NONE',  ( -44.72589015212603414, 164.7311077213657597, 273.2327950865263801 ) ) ;
#4713 = ORIENTED_EDGE ( 'NONE', *, *, #5675, .T. ) ;
#4714 = CARTESIAN_POINT ( 'NONE',  ( 41.12105953731187924, 72.00000000000000000, 86.47576806556189410 ) ) ;
#4715 = AXIS2_PLACEMENT_3D ( 'NONE', #11818, #13536, #15279 ) ;
#4716 = CARTESIAN_POINT ( 'NONE',  ( -88.16990797496626442, 88.76523295132392377, 52.31899320048508883 ) ) ;
#4717 = CARTESIAN_POINT ( 'NONE',  ( -38.68617183816869698, 163.9153776386440882, 273.1592279730091377 ) ) ;
#4718 = CARTESIAN_POINT ( 'NONE',  ( -53.06372157685608215, 189.4876967392748952, -92.30163321429982659 ) ) ;
#4719 = EDGE_CURVE ( 'NONE', #3399, #10079, #4368, .T. ) ;
#4720 = ORIENTED_EDGE ( 'NONE', *, *, #1773, .T. ) ;
#4721 = CIRCLE ( 'NONE', #12461, 2.000000000000001776 ) ;
#4722 = SPHERICAL_SURFACE ( 'NONE', #4395, 2.000000000000000000 ) ;
#4723 = DIRECTION ( 'NONE',  ( -0.01292394549866739996, -0.005513023399721131770, -0.9999012842304692006 ) ) ;
#4724 = CARTESIAN_POINT ( 'NONE',  ( 88.44888535621197434, 80.14369956782289250, -31.98268552584476154 ) ) ;
#4725 = CARTESIAN_POINT ( 'NONE',  ( 86.24279638190516550, 84.99999999999997158, -1.114707239275309458 ) ) ;
#4726 = CARTESIAN_POINT ( 'NONE',  ( -14.07506098016042095, 147.3047514226848023, 276.9331026295720335 ) ) ;
#4727 = EDGE_CURVE ( 'NONE', #8741, #17624, #3334, .T. ) ;
#4728 = EDGE_LOOP ( 'NONE', ( #615, #8980, #21413 ) ) ;
#4729 =( NAMED_UNIT ( * ) PLANE_ANGLE_UNIT ( ) SI_UNIT ( $, .RADIAN. ) );
#4730 = SURFACE_STYLE_FILL_AREA ( #15342 ) ;
#4731 =( BOUNDED_CURVE ( )  B_SPLINE_CURVE ( 3, ( #20272, #20728, #1558, #18996 ),
 .UNSPECIFIED., .F., .T. ) 
 B_SPLINE_CURVE_WITH_KNOTS ( ( 4, 4 ),
 ( 0.000000000000000000, 1.570796326794896558 ),
 .UNSPECIFIED. ) 
 CURVE ( )  GEOMETRIC_REPRESENTATION_ITEM ( )  RATIONAL_B_SPLINE_CURVE ( ( 1.000000000000000000, 0.8047378541243649375, 0.8047378541243649375, 1.000000000000000000 ) ) 
 REPRESENTATION_ITEM ( '' )  );
#4732 = CARTESIAN_POINT ( 'NONE',  ( -64.00981946984995830, 100.1573520573350464, 77.02845195036117332 ) ) ;
#4733 = ORIENTED_EDGE ( 'NONE', *, *, #18206, .T. ) ;
#4734 = CARTESIAN_POINT ( 'NONE',  ( -9.262501379667067880, 187.9054813056602029, 276.0764209250423278 ) ) ;
#4735 = VERTEX_POINT ( 'NONE', #3234 ) ;
#4736 = CARTESIAN_POINT ( 'NONE',  ( -88.73563860332647835, 70.69168859156255280, 62.81961162809064803 ) ) ;
#4737 = EDGE_CURVE ( 'NONE', #13016, #13554, #19021, .T. ) ;
#4738 = VECTOR ( 'NONE', #13774, 1000.000000000000000 ) ;
#4740 = ORIENTED_EDGE ( 'NONE', *, *, #19361, .F. ) ;
#4739 = ORIENTED_EDGE ( 'NONE', *, *, #7083, .F. ) ;
#4741 = FILL_AREA_STYLE ('',( #22083 ) ) ;
#4742 = FACE_BOUND ( 'NONE', #13500, .T. ) ;
#4743 = CARTESIAN_POINT ( 'NONE',  ( -106.1636641531658398, 79.04398536104955042, 28.79715981783285628 ) ) ;
#4744 = FACE_OUTER_BOUND ( 'NONE', #3889, .T. ) ;
#4745 = CARTESIAN_POINT ( 'NONE',  ( 16.00248264617906457, 188.1407795356557529, 275.7525171823001529 ) ) ;
#4746 = ORIENTED_EDGE ( 'NONE', *, *, #10972, .F. ) ;
#4747 = DIRECTION ( 'NONE',  ( -1.000000000000000000, 0.000000000000000000, 1.458023040593674599E-16 ) ) ;
#4748 = LINE ( 'NONE', #20612, #9569 ) ;
#4749 = CARTESIAN_POINT ( 'NONE',  ( 4.376210989365964643, 81.97459999999998104, -92.29796090835097289 ) ) ;
#4750 = DIRECTION ( 'NONE',  ( -0.01292394549866750231, -0.005513023399722823126, -0.9999012842304692006 ) ) ;
#4751 = AXIS2_PLACEMENT_3D ( 'NONE', #15611, #17000, #1263 ) ;
#4752 = CARTESIAN_POINT ( 'NONE',  ( 90.47544334248004816, 78.08471258854567054, -32.66922098773476790 ) ) ;
#4753 = EDGE_CURVE ( 'NONE', #8542, #11891, #2898, .T. ) ;
#4754 = DIRECTION ( 'NONE',  ( -0.009188991635466048358, 0.7031977391749438810, -0.7109349492407661675 ) ) ;
#4755 = ORIENTED_EDGE ( 'NONE', *, *, #17100, .F. ) ;
#4756 = VERTEX_POINT ( 'NONE', #18365 ) ;
#4757 = CARTESIAN_POINT ( 'NONE',  ( -20.57109388430227881, 136.7551719540686008, -44.05520973278501629 ) ) ;
#4758 = AXIS2_PLACEMENT_3D ( 'NONE', #12395, #4090, #19700 ) ;
#4759 = CARTESIAN_POINT ( 'NONE',  ( -11.19281454843939194, 155.5569384583423300, 101.2152518466410243 ) ) ;
#4760 = ORIENTED_EDGE ( 'NONE', *, *, #1478, .T. ) ;
#4761 = CARTESIAN_POINT ( 'NONE',  ( -6.335846763728186559, 188.7674449536879706, 275.9742639064239142 ) ) ;
#4762 = EDGE_LOOP ( 'NONE', ( #18542, #965, #20284, #14850 ) ) ;
#4763 = PRODUCT_DEFINITION_SHAPE ( 'NONE', 'NONE',  #22673 ) ;
#4764 = AXIS2_PLACEMENT_3D ( 'NONE', #844, #5754, #14638 ) ;
#4765 = DIRECTION ( 'NONE',  ( -1.000000000000000000, 0.000000000000000000, 0.000000000000000000 ) ) ;
#4766 = VECTOR ( 'NONE', #1983, 999.9999999999998863 ) ;
#4767 = PRODUCT_DEFINITION_FORMATION_WITH_SPECIFIED_SOURCE ( 'ANY', '', #5858, .NOT_KNOWN. ) ;
#4768 = CARTESIAN_POINT ( 'NONE',  ( -4.135966696445571245, 326.8123805703096423, 307.5996468166270006 ) ) ;
#4769 = CARTESIAN_POINT ( 'NONE',  ( -9.829263477007989636, 187.6861072963453125, 321.1599754959502775 ) ) ;
#4770 = VECTOR ( 'NONE', #20499, 1000.000000000000227 ) ;
#4771 = CARTESIAN_POINT ( 'NONE',  ( 15.78165906541865304, 186.0656686932232446, 322.5043251233448700 ) ) ;
#4772 = EDGE_CURVE ( 'NONE', #12735, #14385, #5444, .T. ) ;
#4773 = DIRECTION ( 'NONE',  ( -0.009760756503428009989, 0.9999378516499564107, -0.005387065077611111891 ) ) ;
#4774 = EDGE_CURVE ( 'NONE', #5658, #15608, #15761, .T. ) ;
#4775 = ORIENTED_EDGE ( 'NONE', *, *, #4774, .T. ) ;
#4776 = CARTESIAN_POINT ( 'NONE',  ( 106.2089377515399065, 77.12912189496647386, 28.62973177816241588 ) ) ;
#4777 = EDGE_CURVE ( 'NONE', #10313, #3247, #3978, .T. ) ;
#4779 = DIRECTION ( 'NONE',  ( 0.000000000000000000, 0.000000000000000000, -1.000000000000000000 ) ) ;
#4778 = CARTESIAN_POINT ( 'NONE',  ( -45.36474727608072044, 165.8559883853732515, 234.9810740996818481 ) ) ;
#4780 = CIRCLE ( 'NONE', #4055, 2.000000000000001332 ) ;
#4781 = ORIENTED_EDGE ( 'NONE', *, *, #13973, .F. ) ;
#4782 = CARTESIAN_POINT ( 'NONE',  ( -56.11559749965279309, 143.5880916635282176, 107.4801945902891021 ) ) ;
#4783 = ORIENTED_EDGE ( 'NONE', *, *, #8641, .F. ) ;
#4784 = VERTEX_POINT ( 'NONE', #2038 ) ;
#4785 = DIRECTION ( 'NONE',  ( -0.01292394549866745720, -0.005513023399720816918, -0.9999012842304692006 ) ) ;
#4786 = LINE ( 'NONE', #2965, #4738 ) ;
#4787 = AXIS2_PLACEMENT_3D ( 'NONE', #9673, #14864, #11385 ) ;
#4788 = CARTESIAN_POINT ( 'NONE',  ( -12.82378010018955550, 184.2676410047889703, 320.0244981536045543 ) ) ;
#4789 = CARTESIAN_POINT ( 'NONE',  ( -89.18698784711349958, 88.49522953700143546, 50.47455866862448204 ) ) ;
#4790 = ORIENTED_EDGE ( 'NONE', *, *, #7603, .T. ) ;
#4791 = CARTESIAN_POINT ( 'NONE',  ( -1.362186893977295590E-13, 20.00000000000000000, 9.999999999999994671 ) ) ;
#4792 = AXIS2_PLACEMENT_3D ( 'NONE', #9380, #7645, #2490 ) ;
#4793 = CARTESIAN_POINT ( 'NONE',  ( -64.13742787616538976, 91.41757367590341232, 67.15563026703152616 ) ) ;
#4794 = DIRECTION ( 'NONE',  ( 0.9999164797902017066, 2.001050586450178931E-22, -0.01292414190464131508 ) ) ;
#4795 = ORIENTED_EDGE ( 'NONE', *, *, #12097, .T. ) ;
#4796 = CIRCLE ( 'NONE', #7776, 7.499999999999991118 ) ;
#4797 = CARTESIAN_POINT ( 'NONE',  ( -50.59241450076314095, 108.3707227317548103, -45.51087538574415703 ) ) ;
#4798 = VERTEX_POINT ( 'NONE', #19368 ) ;
#4799 = FACE_OUTER_BOUND ( 'NONE', #7841, .T. ) ;
#4800 = FACE_OUTER_BOUND ( 'NONE', #22230, .T. ) ;
#4801 = ORIENTED_EDGE ( 'NONE', *, *, #20623, .T. ) ;
#4802 = VECTOR ( 'NONE', #22498, 1000.000000000000114 ) ;
#4803 = CARTESIAN_POINT ( 'NONE',  ( -5.788558211672063969, 70.69320546282760631, -88.06740927887889825 ) ) ;
#4804 = DIRECTION ( 'NONE',  ( -0.01292394549866741904, -0.005513023399721091004, -0.9999012842304693116 ) ) ;
#4805 = ORIENTED_EDGE ( 'NONE', *, *, #585, .F. ) ;
#4806 = CARTESIAN_POINT ( 'NONE',  ( -89.97609184686128003, 87.77209961377428726, 50.92695616138752257 ) ) ;
#4807 = CIRCLE ( 'NONE', #10699, 2.499999999999988010 ) ;
#4808 = ORIENTED_EDGE ( 'NONE', *, *, #13595, .T. ) ;
#4809 = DIRECTION ( 'NONE',  ( 1.000000000000000000, 0.000000000000000000, -1.387778780781444413E-14 ) ) ;
#4810 = DIRECTION ( 'NONE',  ( 0.4397038457472354778, 0.000000000000000000, -0.8981428216242066664 ) ) ;
#4811 = DIRECTION ( 'NONE',  ( 0.000000000000000000, 0.000000000000000000, 1.000000000000000000 ) ) ;
#4812 = CARTESIAN_POINT ( 'NONE',  ( -52.61410854296865836, 118.5884715842524457, 107.5727741673942148 ) ) ;
#4813 = EDGE_CURVE ( 'NONE', #8554, #18838, #3634, .T. ) ;
#4814 = VERTEX_POINT ( 'NONE', #14928 ) ;
#4815 = FACE_BOUND ( 'NONE', #13111, .T. ) ;
#4816 = CARTESIAN_POINT ( 'NONE',  ( -51.46461399095765898, 114.4383923424130813, 171.3466661713325720 ) ) ;
#4817 = VECTOR ( 'NONE', #14915, 1000.000000000000114 ) ;
#4818 = ORIENTED_EDGE ( 'NONE', *, *, #18267, .F. ) ;
#4819 = CARTESIAN_POINT ( 'NONE',  ( 48.70718024533385915, 95.27297528470670329, -45.18526822691359257 ) ) ;
#4820 = DIRECTION ( 'NONE',  ( -0.01292394549866741384, -0.005513023399720269613, -0.9999012842304692006 ) ) ;
#4821 = ORIENTED_EDGE ( 'NONE', *, *, #10753, .F. ) ;
#4822 = AXIS2_PLACEMENT_3D ( 'NONE', #18602, #8595, #2866 ) ;
#4823 = DIRECTION ( 'NONE',  ( 0.9999164797902015955, 6.965998958219364448E-18, -0.01292414190464157182 ) ) ;
#4824 = EDGE_CURVE ( 'NONE', #6959, #19631, #5802, .T. ) ;
#4825 = CARTESIAN_POINT ( 'NONE',  ( -88.16428333377376703, 88.34422939329346036, 52.84359960540316337 ) ) ;
#4826 = CONICAL_SURFACE ( 'NONE', #10363, 6.000000000000000888, 0.7853981633974509435 ) ;
#4827 = ORIENTED_EDGE ( 'NONE', *, *, #21735, .F. ) ;
#4828 = LINE ( 'NONE', #13815, #54 ) ;
#4829 = CARTESIAN_POINT ( 'NONE',  ( 64.42123688909094881, 144.7550503794368524, -45.19786229828635271 ) ) ;
#4830 = CARTESIAN_POINT ( 'NONE',  ( -19.94685613197333751, 88.10794472606065142, -76.88480816673754248 ) ) ;
#4831 = DIRECTION ( 'NONE',  ( 0.01292394549866731843, 0.005513023399720594006, 0.9999012842304693116 ) ) ;
#4832 = AXIS2_PLACEMENT_3D ( 'NONE', #10395, #10509, #12356 ) ;
#4833 = DIRECTION ( 'NONE',  ( -7.176269450075762180E-19, 1.000000000000000000, -5.550596000020001457E-17 ) ) ;
#4834 = CARTESIAN_POINT ( 'NONE',  ( 51.12138307655921921, 113.4816418249608319, -44.85353068836323587 ) ) ;
#4835 = CIRCLE ( 'NONE', #3752, 1.999999999999997335 ) ;
#4836 = CIRCLE ( 'NONE', #19525, 102.4713510550357398 ) ;
#4837 = DIRECTION ( 'NONE',  ( -0.9999464000778708339, -1.417269118681738834E-05, 0.01035358732233848493 ) ) ;
#4838 = EDGE_LOOP ( 'NONE', ( #6412, #8577, #19529, #18955 ) ) ;
#4839 = ORIENTED_EDGE ( 'NONE', *, *, #15442, .T. ) ;
#4840 = DIRECTION ( 'NONE',  ( -2.025474946048326158E-22, 1.000000000000000000, -1.876735158486679638E-22 ) ) ;
#4841 = FACE_OUTER_BOUND ( 'NONE', #19750, .T. ) ;
#4842 = LINE ( 'NONE', #6480, #6143 ) ;
#4843 = LINE ( 'NONE', #17061, #3346 ) ;
#4844 = ADVANCED_FACE ( 'NONE', ( #5928 ), #9868, .F. ) ;
#4845 = ADVANCED_FACE ( 'NONE', ( #10173 ), #404, .F. ) ;
#4846 = CARTESIAN_POINT ( 'NONE',  ( -146.5000000000000000, 0.000000000000000000, 2.081668171172168513E-14 ) ) ;
#4847 = DIRECTION ( 'NONE',  ( 0.000000000000000000, 0.000000000000000000, 1.000000000000000000 ) ) ;
#4848 = CONICAL_SURFACE ( 'NONE', #15890, 3.399999999999991918, 1.029744258676652313 ) ;
#4849 = FACE_OUTER_BOUND ( 'NONE', #16653, .T. ) ;
#4850 =( REPRESENTATION_RELATIONSHIP ('NONE','NONE', #11808, #14914 ) REPRESENTATION_RELATIONSHIP_WITH_TRANSFORMATION ( #5817 )SHAPE_REPRESENTATION_RELATIONSHIP( ) );
#4851 = CARTESIAN_POINT ( 'NONE',  ( -66.75225376373553843, 145.1029152106950164, 19.60063580020017326 ) ) ;
#4852 = ORIENTED_EDGE ( 'NONE', *, *, #22479, .T. ) ;
#4854 = CARTESIAN_POINT ( 'NONE',  ( -9.985275337145829155, 186.6414244315945155, 277.9386990328198408 ) ) ;
#4853 = VECTOR ( 'NONE', #14488, 1000.000000000000114 ) ;
#4855 = ORIENTED_EDGE ( 'NONE', *, *, #20081, .F. ) ;
#4856 = CIRCLE ( 'NONE', #466, 10.00000000000000355 ) ;
#4857 = EDGE_CURVE ( 'NONE', #15892, #21893, #571, .T. ) ;
#4858 = CARTESIAN_POINT ( 'NONE',  ( -20.14020152772452477, -0.1201756712316815051, -10.71788091538852861 ) ) ;
#4859 = ORIENTED_EDGE ( 'NONE', *, *, #12599, .F. ) ;
#4860 = EDGE_CURVE ( 'NONE', #1365, #13728, #8249, .T. ) ;
#4861 = DIRECTION ( 'NONE',  ( -0.003413786507415475339, 0.9644842718275420390, -0.2641182225045781706 ) ) ;
#4862 = CARTESIAN_POINT ( 'NONE',  ( -6.632709584382701529, 81.44153265534507113, -81.62749566292762893 ) ) ;
#4863 = CARTESIAN_POINT ( 'NONE',  ( -108.6051929143322781, 76.36431273661725072, 17.61389195241277150 ) ) ;
#4864 = DIRECTION ( 'NONE',  ( 0.000000000000000000, 0.000000000000000000, 1.000000000000000000 ) ) ;
#4865 = CARTESIAN_POINT ( 'NONE',  ( 18.37741161651380395, 185.7965308539349110, 276.6192911305356574 ) ) ;
#4866 = DIRECTION ( 'NONE',  ( 1.000000000000000000, -0.000000000000000000, 1.224646799147353207E-16 ) ) ;
#4867 = CARTESIAN_POINT ( 'NONE',  ( -44.23502202816609241, 168.8246939296723497, 59.47570800643972433 ) ) ;
#4868 = CARTESIAN_POINT ( 'NONE',  ( 45.73105848731719192, 168.8134312302534283, 56.26981079935081453 ) ) ;
#4869 = AXIS2_PLACEMENT_3D ( 'NONE', #10637, #14107, #21088 ) ;
#4870 = CARTESIAN_POINT ( 'NONE',  ( -4.113941462729931331, 165.7267928694881789, 296.7047562922618908 ) ) ;
#4871 = CIRCLE ( 'NONE', #1576, 8.000000000000005329 ) ;
#4872 = EDGE_CURVE ( 'NONE', #8679, #13676, #15384, .T. ) ;
#4873 = FACE_OUTER_BOUND ( 'NONE', #15891, .T. ) ;
#4874 = ORIENTED_EDGE ( 'NONE', *, *, #1920, .F. ) ;
#4875 = CARTESIAN_POINT ( 'NONE',  ( 91.62437796271727564, 72.00000000000000000, 60.86849236629024773 ) ) ;
#4876 = VERTEX_POINT ( 'NONE', #22114 ) ;
#4877 = ORIENTED_EDGE ( 'NONE', *, *, #19305, .F. ) ;
#4878 = CARTESIAN_POINT ( 'NONE',  ( -37.14184569576254091, 95.72081062788153361, 84.97917966163161907 ) ) ;
#4879 = CARTESIAN_POINT ( 'NONE',  ( 163.9999999999992610, 18.00000000000000355, -53.76161406891485228 ) ) ;
#4880 = ORIENTED_EDGE ( 'NONE', *, *, #9948, .F. ) ;
#4881 = AXIS2_PLACEMENT_3D ( 'NONE', #11565, #21862, #1949 ) ;
#4882 = CARTESIAN_POINT ( 'NONE',  ( 67.23320572660466610, 192.1022009597330680, 17.60971032628828681 ) ) ;
#4883 = VERTEX_POINT ( 'NONE', #22334 ) ;
#4884 = ADVANCED_FACE ( 'NONE', ( #13430, #20640 ), #17320, .F. ) ;
#4885 = AXIS2_PLACEMENT_3D ( 'NONE', #18779, #3936, #7390 ) ;
#4886 = AXIS2_PLACEMENT_3D ( 'NONE', #7294, #75, #10418 ) ;
#4887 = CARTESIAN_POINT ( 'NONE',  ( -70.78416300399055672, 71.33159407511109862, -84.19980244608493081 ) ) ;
#4888 = EDGE_CURVE ( 'NONE', #17417, #17190, #17975, .T. ) ;
#4889 = PRODUCT_DEFINITION_CONTEXT ( 'detailed design', #19944, 'design' ) ;
#4890 = CARTESIAN_POINT ( 'NONE',  ( 0.000000000000000000, 37.00000000000000711, 0.000000000000000000 ) ) ;
#4891 = CARTESIAN_POINT ( 'NONE',  ( 41.42451162475439475, 125.7553391191873544, -44.79586833841344173 ) ) ;
#4892 = ORIENTED_EDGE ( 'NONE', *, *, #4772, .F. ) ;
#4893 = DIRECTION ( 'NONE',  ( 0.3101392564284309317, 0.9506461370142480494, -0.009250070373105347826 ) ) ;
#4894 = ORIENTED_EDGE ( 'NONE', *, *, #11683, .F. ) ;
#4895 = AXIS2_PLACEMENT_3D ( 'NONE', #1426, #20701, #8405 ) ;
#4896 = AXIS2_PLACEMENT_3D ( 'NONE', #2983, #10001, #17027 ) ;
#4897 = EDGE_CURVE ( 'NONE', #1183, #1264, #12473, .T. ) ;
#4898 = ADVANCED_FACE ( 'NONE', ( #6416 ), #6846, .F. ) ;
#4899 = FACE_OUTER_BOUND ( 'NONE', #7195, .T. ) ;
#4900 = ORIENTED_EDGE ( 'NONE', *, *, #2760, .T. ) ;
#4901 =( NAMED_UNIT ( * ) PLANE_ANGLE_UNIT ( ) SI_UNIT ( $, .RADIAN. ) );
#4902 = CARTESIAN_POINT ( 'NONE',  ( 64.42446510409216387, 113.4816418249608034, -45.02547596916208050 ) ) ;
#4903 = AXIS2_PLACEMENT_3D ( 'NONE', #18282, #599, #3910 ) ;
#4904 = EDGE_LOOP ( 'NONE', ( #3760, #16432, #10968, #1859, #7622, #21982 ) ) ;
#4905 = PLANE ( 'NONE',  #18049 ) ;
#4906 = AXIS2_PLACEMENT_3D ( 'NONE', #16107, #8839, #2971 ) ;
#4907 = PLANE ( 'NONE',  #14706 ) ;
#4908 = CARTESIAN_POINT ( 'NONE',  ( -12.64688860274155324, 109.6831087301383860, 124.2482791415423691 ) ) ;
#4909 = CARTESIAN_POINT ( 'NONE',  ( -11.71322822773759320, 182.7629020050958673, 320.7064967533905246 ) ) ;
#4910 = CARTESIAN_POINT ( 'NONE',  ( 44.31808358225305966, 164.8106407359766763, -53.04939224934937414 ) ) ;
#4911 = CIRCLE ( 'NONE', #3833, 95.00000000000004263 ) ;
#4912 = DIRECTION ( 'NONE',  ( 0.9232306267972774094, 0.000000000000000000, -0.3842462878721227826 ) ) ;
#4913 = CARTESIAN_POINT ( 'NONE',  ( 79.99331838321626265, 55.99999999999999289, -1.033931352371318058 ) ) ;
#4914 = EDGE_CURVE ( 'NONE', #16716, #17834, #1261, .T. ) ;
#4915 = CONTEXT_DEPENDENT_SHAPE_REPRESENTATION ( #1356, #8636 ) ;
#4916 = EDGE_CURVE ( 'NONE', #7484, #19228, #17214, .T. ) ;
#4917 = VECTOR ( 'NONE', #17641, 1000.000000000000000 ) ;
#4918 = ORIENTED_EDGE ( 'NONE', *, *, #20196, .F. ) ;
#4919 = CIRCLE ( 'NONE', #17806, 2.000000000000000000 ) ;
#4920 = DIRECTION ( 'NONE',  ( 0.01292394549866741557, 0.005513023399720270480, 0.9999012842304693116 ) ) ;
#4921 = CARTESIAN_POINT ( 'NONE',  ( 84.52636712416138209, 105.0000000000000000, -71.24109250138926086 ) ) ;
#4922 = DIRECTION ( 'NONE',  ( -0.9999164797902015955, -6.965998958219364448E-18, 0.01292414190464157182 ) ) ;
#4923 = DIRECTION ( 'NONE',  ( -0.9999164797902017066, -2.001050586450178931E-22, 0.01292414190464131508 ) ) ;
#4924 = ORIENTED_EDGE ( 'NONE', *, *, #16418, .F. ) ;
#4925 = DIRECTION ( 'NONE',  ( 2.025474946048326158E-22, -1.000000000000000000, 1.876735158486679638E-22 ) ) ;
#4926 = CARTESIAN_POINT ( 'NONE',  ( -55.72875598653071449, 138.9025232320894077, 164.5272005411160023 ) ) ;
#4927 = ORIENTED_EDGE ( 'NONE', *, *, #13849, .F. ) ;
#4928 = CARTESIAN_POINT ( 'NONE',  ( 49.46305616158914376, 112.8312625773126712, -44.82851053580059641 ) ) ;
#4929 = VERTEX_POINT ( 'NONE', #3171 ) ;
#4930 = CARTESIAN_POINT ( 'NONE',  ( -5.135453193612369738, 87.00000000000001421, -93.02909119787791781 ) ) ;
#4931 = DIRECTION ( 'NONE',  ( -0.9999164797902015955, -2.045733645417851287E-15, 0.01292414190464156835 ) ) ;
#4932 = FACE_OUTER_BOUND ( 'NONE', #8930, .T. ) ;
#4933 = FACE_OUTER_BOUND ( 'NONE', #5937, .T. ) ;
#4934 = CARTESIAN_POINT ( 'NONE',  ( 0.000000000000000000, 0.000000000000000000, -83.99999999999998579 ) ) ;
#4935 = EDGE_LOOP ( 'NONE', ( #10831, #2532, #11587, #5031 ) ) ;
#4936 = CARTESIAN_POINT ( 'NONE',  ( 49.18241401050376993, 95.63349031005608936, -45.79074433281897427 ) ) ;
#4937 = DIRECTION ( 'NONE',  ( 0.9999164797902017066, 2.001050586450180811E-22, -0.01292414190464045119 ) ) ;
#4938 = ORIENTED_EDGE ( 'NONE', *, *, #11943, .F. ) ;
#4939 = DIRECTION ( 'NONE',  ( -7.125109674025824596E-05, 0.9999848031710253382, -0.005512562950848693549 ) ) ;
#4940 = CARTESIAN_POINT ( 'NONE',  ( -90.15048749786897986, 87.28265959684701158, 51.22645766322034433 ) ) ;
#4941 = AXIS2_PLACEMENT_3D ( 'NONE', #346, #238, #5498 ) ;
#4943 = EDGE_LOOP ( 'NONE', ( #4138, #10912 ) ) ;
#4942 = VERTEX_POINT ( 'NONE', #15607 ) ;
#4944 = ORIENTED_EDGE ( 'NONE', *, *, #18250, .T. ) ;
#4945 = CARTESIAN_POINT ( 'NONE',  ( -9.065023647928146744, 109.7167603697149474, 130.3064260814875013 ) ) ;
#4946 = CARTESIAN_POINT ( 'NONE',  ( -45.96219963993937796, 168.0879242961143518, -74.15276576609245751 ) ) ;
#4947 = CARTESIAN_POINT ( 'NONE',  ( -4.071909468699204560, 86.19497019983103314, -75.00673844656712674 ) ) ;
#4948 = DIRECTION ( 'NONE',  ( -0.9999164797902015955, 0.000000000000000000, 0.01292414190464162733 ) ) ;
#4949 = DIRECTION ( 'NONE',  ( -0.9999164797902017066, -2.775557561562891351E-15, 0.01292414190464108437 ) ) ;
#4950 = FACE_OUTER_BOUND ( 'NONE', #16362, .T. ) ;
#4951 = ORIENTED_EDGE ( 'NONE', *, *, #22283, .F. ) ;
#4952 = ORIENTED_EDGE ( 'NONE', *, *, #1542, .F. ) ;
#4953 = ADVANCED_BREP_SHAPE_REPRESENTATION ( '', ( #2209, #6292 ), #6306 ) ;
#4954 = ORIENTED_EDGE ( 'NONE', *, *, #794, .T. ) ;
#4955 = DIRECTION ( 'NONE',  ( -0.9999164797902017066, -9.297033629063200522E-18, 0.01292414190464145386 ) ) ;
#4956 = DIRECTION ( 'NONE',  ( -0.000000000000000000, -1.000000000000000000, -0.000000000000000000 ) ) ;
#4957 = CARTESIAN_POINT ( 'NONE',  ( 91.93574473583117879, 79.05185923607193388, -28.63941780214908661 ) ) ;
#4958 = DIRECTION ( 'NONE',  ( -5.440186201345738641E-18, -1.000000000000000000, -1.334940939666364181E-17 ) ) ;
#4959 = FACE_OUTER_BOUND ( 'NONE', #18652, .T. ) ;
#4960 = ORIENTED_EDGE ( 'NONE', *, *, #12149, .F. ) ;
#4961 = AXIS2_PLACEMENT_3D ( 'NONE', #2964, #14838, #21788 ) ;
#4962 = PRODUCT_DEFINITION_SHAPE ( 'NONE', 'NONE',  #22674 ) ;
#4963 = DIRECTION ( 'NONE',  ( 0.000000000000000000, 0.000000000000000000, 1.000000000000000000 ) ) ;
#4964 = ORIENTED_EDGE ( 'NONE', *, *, #20279, .T. ) ;
#4965 = VERTEX_POINT ( 'NONE', #18685 ) ;
#4966 = ORIENTED_EDGE ( 'NONE', *, *, #14712, .T. ) ;
#4967 = ADVANCED_FACE ( 'NONE', ( #20854 ), #8244, .F. ) ;
#4968 = DIRECTION ( 'NONE',  ( -7.125109674161246868E-05, 0.9999848031710253382, -0.005512562950850155054 ) ) ;
#4969 = EDGE_CURVE ( 'NONE', #17515, #7720, #7301, .T. ) ;
#4970 = EDGE_CURVE ( 'NONE', #19436, #7332, #18010, .T. ) ;
#4971 = FACE_OUTER_BOUND ( 'NONE', #19893, .T. ) ;
#4972 = CARTESIAN_POINT ( 'NONE',  ( 51.42288047930750139, 166.7281037598372961, 233.7252641129099970 ) ) ;
#4973 = ADVANCED_FACE ( 'NONE', ( #426 ), #3519, .T. ) ;
#4974 = AXIS2_PLACEMENT_3D ( 'NONE', #10223, #6873, #13791 ) ;
#4975 = CARTESIAN_POINT ( 'NONE',  ( 86.24813375828298945, 75.00000000000002842, -0.7017644970498472246 ) ) ;
#4976 = DIRECTION ( 'NONE',  ( 0.009760756503428003050, -0.9999378516499565217, 0.005387065077610373766 ) ) ;
#4977 = ORIENTED_EDGE ( 'NONE', *, *, #15833, .F. ) ;
#4978 = DIRECTION ( 'NONE',  ( 0.01292394549866740169, 0.005513023399719847208, 0.9999012842304693116 ) ) ;
#4979 = LINE ( 'NONE', #20382, #8104 ) ;
#4980 = CARTESIAN_POINT ( 'NONE',  ( 4.182528737366220106, 166.7840834110302808, 323.5943587238651276 ) ) ;
#4981 = FACE_OUTER_BOUND ( 'NONE', #2499, .T. ) ;
#4982 = CARTESIAN_POINT ( 'NONE',  ( -50.96731222690930707, 189.5912335953706531, -73.54703356252615265 ) ) ;
#4983 = APPLICATION_CONTEXT ( 'automotive_design' ) ;
#4984 = EDGE_CURVE ( 'NONE', #18610, #134, #731, .T. ) ;
#4985 = DIRECTION ( 'NONE',  ( 7.125109674161246868E-05, -0.9999848031710252272, 0.005512562950850154186 ) ) ;
#4986 = EDGE_CURVE ( 'NONE', #2150, #14146, #6216, .T. ) ;
#4987 = CYLINDRICAL_SURFACE ( 'NONE', #16916, 2.000000000000004885 ) ;
#4988 = CARTESIAN_POINT ( 'NONE',  ( -8.689953299324470137, 185.3004383898032188, 305.1731502674360286 ) ) ;
#4989 = ORIENTED_EDGE ( 'NONE', *, *, #21416, .F. ) ;
#4990 = CARTESIAN_POINT ( 'NONE',  ( -91.22751156961061270, 80.31838830481380853, -30.16368815799732417 ) ) ;
#4991 = ORIENTED_EDGE ( 'NONE', *, *, #14311, .F. ) ;
#4992 = AXIS2_PLACEMENT_3D ( 'NONE', #4354, #18392, #19745 ) ;
#4993 = ADVANCED_FACE ( 'NONE', ( #80, #5344 ), #3747, .F. ) ;
#4994 = B_SPLINE_CURVE_WITH_KNOTS ( 'NONE', 3,
 ( #15322, #1189, #4494, #16811 ),
 .UNSPECIFIED., .F., .F.,
 ( 4, 4 ),
 ( 0.000000000000000000, 0.001461243987307916069 ),
 .UNSPECIFIED. ) ;
#4995 = CARTESIAN_POINT ( 'NONE',  ( 13.02962957137955335, 190.4272972286120478, 320.8494027134000817 ) ) ;
#4996 = EDGE_CURVE ( 'NONE', #22603, #20787, #15838, .T. ) ;
#4997 =( BOUNDED_SURFACE ( )  B_SPLINE_SURFACE ( 3, 2, ( 
 ( #1376, #22237, #6529 ),
 ( #20524, #4909, #4788 ),
 ( #11940, #18926, #10205 ),
 ( #14356, #3640, #9029 ),
 ( #211, #9148, #19818 ),
 ( #21326, #5469, #21213 ),
 ( #12734, #3876, #16199 ),
 ( #12505, #1935, #7314 ),
 ( #15854, #5357, #17914 ),
 ( #12397, #14238, #8925 ),
 ( #7207, #12842, #10544 ),
 ( #10993, #323, #10887 ),
 ( #17563, #2148, #15972 ),
 ( #21101, #7437, #16082 ),
 ( #5594, #17810, #19491 ),
 ( #12629, #19376, #7555 ),
 ( #19701, #2044, #1814 ),
 ( #14477, #21442, #439 ),
 ( #8800, #5702, #3766 ),
 ( #10654, #3970, #19603 ),
 ( #18023, #2271, #10778 ),
 ( #9270, #16317, #557 ),
 ( #97, #14582, #21538 ),
 ( #5808, #7093, #14124 ),
 ( #17689, #11236, #9384 ),
 ( #18241, #21987, #14695 ),
 ( #18340, #7778, #9624 ),
 ( #15153, #21763, #9841 ),
 ( #11459, #13087, #21647 ),
 ( #16861, #11574, #5936 ),
 ( #4429, #14932, #20054 ),
 ( #6404, #16652, #16759 ),
 ( #2394, #16421, #6288 ),
 ( #18466, #902, #1125 ),
 ( #2731, #13313, #9744 ),
 ( #18573, #2496, #8120 ),
 ( #20283, #4311, #7995 ),
 ( #9495, #1007, #2834 ),
 ( #15033, #11340, #13422 ),
 ( #4546, #16530, #4208 ),
 ( #22102, #4091, #7892 ),
 ( #11123, #21871, #18143 ),
 ( #664, #12973, #7652 ),
 ( #19938, #782, #14815 ),
 ( #6058, #2613, #6168 ),
 ( #13193, #20161, #15267 ),
 ( #3396, #22216, #1352 ),
 ( #4988, #17091, #22644 ),
 ( #20392, #11682, #3159 ),
 ( #8553, #16986, #10408 ),
 ( #15594, #18797, #13752 ),
 ( #12016, #8329, #6940 ),
 ( #4651, #18673, #10178 ),
 ( #8658, #15702, #1247 ) ),
 .UNSPECIFIED., .F., .F., .T. ) 
 B_SPLINE_SURFACE_WITH_KNOTS ( ( 4, 2, 2, 2, 2, 2, 2, 2, 2, 2, 2, 2, 2, 2, 2, 2, 2, 2, 2, 2, 2, 2, 2, 2, 2, 2, 4 ),
 ( 3, 3 ),
 ( 0.1301284894805934678, 0.1318527056069465075, 0.1335769217332995473, 0.1353011378596525871, 0.1361632459228291070, 0.1370253539860056269, 0.1387495701123586667, 0.1396116781755351866, 0.1404737862387117064, 0.1413358943018882263, 0.1421980023650647462, 0.1430601104282412661, 0.1439222184914177860, 0.1456464346177708258, 0.1465085426809473457, 0.1473706507441238656, 0.1490948668704769053, 0.1499569749336534252, 0.1508190829968299451, 0.1542675152495360247, 0.1551296233127125446, 0.1559917313758890645, 0.1568538394390656121, 0.1572848934706538859, 0.1573926569785509544, 0.1575004204864480228, 0.1577159475022421320 ),
 ( 0.000000000000000000, 1.000000000000000000 ),
 .UNSPECIFIED. ) 
 GEOMETRIC_REPRESENTATION_ITEM ( )  RATIONAL_B_SPLINE_SURFACE ( (
 ( 1.000000000000000000, 0.8227386401542207128, 1.000000000000000000),
 ( 1.000000000000000000, 0.8333712125770807999, 1.000000000000000000),
 ( 1.000000000000000000, 0.8437848470051855232, 1.000000000000000000),
 ( 1.000000000000000000, 0.8640507908242766044, 1.000000000000000000),
 ( 1.000000000000000000, 0.8738632290070461606, 1.000000000000000000),
 ( 1.000000000000000000, 0.8923321234614439712, 1.000000000000000000),
 ( 1.000000000000000000, 0.9010134951843085105, 1.000000000000000000),
 ( 1.000000000000000000, 0.9129850007871143092, 1.000000000000000000),
 ( 1.000000000000000000, 0.9168115705809977145, 1.000000000000000000),
 ( 1.000000000000000000, 0.9241129455457998132, 1.000000000000000000),
 ( 1.000000000000000000, 0.9275997298644027556, 1.000000000000000000),
 ( 1.000000000000000000, 0.9371813536878720319, 1.000000000000000000),
 ( 1.000000000000000000, 0.9425342029318131143, 1.000000000000000000),
 ( 1.000000000000000000, 0.9487217190514500853, 1.000000000000000000),
 ( 1.000000000000000000, 0.9504219373548455918, 1.000000000000000000),
 ( 1.000000000000000000, 0.9530138574316157074, 1.000000000000000000),
 ( 1.000000000000000000, 0.9539189288212627238, 1.000000000000000000),
 ( 1.000000000000000000, 0.9548931618690527090, 1.000000000000000000),
 ( 1.000000000000000000, 0.9549507483037429356, 1.000000000000000000),
 ( 1.000000000000000000, 0.9541752437097101858, 1.000000000000000000),
 ( 1.000000000000000000, 0.9533611900843690368, 1.000000000000000000),
 ( 1.000000000000000000, 0.9509603907209587259, 1.000000000000000000),
 ( 1.000000000000000000, 0.9493731739221451527, 1.000000000000000000),
 ( 1.000000000000000000, 0.9454412650859107536, 1.000000000000000000),
 ( 1.000000000000000000, 0.9431063129023899982, 1.000000000000000000),
 ( 1.000000000000000000, 0.9353430921237518847, 1.000000000000000000),
 ( 1.000000000000000000, 0.9290748369521870664, 1.000000000000000000),
 ( 1.000000000000000000, 0.9182885162027015769, 1.000000000000000000),
 ( 1.000000000000000000, 0.9144642180539555021, 1.000000000000000000),
 ( 1.000000000000000000, 0.9065214887599388760, 1.000000000000000000),
 ( 1.000000000000000000, 0.9023952855941976825, 1.000000000000000000),
 ( 1.000000000000000000, 0.8895549064154443242, 1.000000000000000000),
 ( 1.000000000000000000, 0.8803896720082297067, 1.000000000000000000),
 ( 1.000000000000000000, 0.8659833981722644403, 1.000000000000000000),
 ( 1.000000000000000000, 0.8610623523000291435, 1.000000000000000000),
 ( 1.000000000000000000, 0.8509715058880433780, 1.000000000000000000),
 ( 1.000000000000000000, 0.8457963385677346180, 1.000000000000000000),
 ( 1.000000000000000000, 0.8197273272024717672, 1.000000000000000000),
 ( 1.000000000000000000, 0.7979877476287833282, 1.000000000000000000),
 ( 1.000000000000000000, 0.7710357334748190183, 1.000000000000000000),
 ( 1.000000000000000000, 0.7656985913657583520, 1.000000000000000000),
 ( 1.000000000000000000, 0.7550404585215626518, 1.000000000000000000),
 ( 1.000000000000000000, 0.7497880368474888479, 1.000000000000000000),
 ( 1.000000000000000000, 0.7395325035323125906, 1.000000000000000000),
 ( 1.000000000000000000, 0.7345293846932524628, 1.000000000000000000),
 ( 1.000000000000000000, 0.7272879817929819302, 1.000000000000000000),
 ( 1.000000000000000000, 0.7249181014104938425, 1.000000000000000000),
 ( 1.000000000000000000, 0.7220190359316460693, 1.000000000000000000),
 ( 1.000000000000000000, 0.7214423886269636377, 1.000000000000000000),
 ( 1.000000000000000000, 0.7202956422195359032, 1.000000000000000000),
 ( 1.000000000000000000, 0.7204858121524565506, 1.000000000000000000),
 ( 1.000000000000000000, 0.7203839998076618789, 1.000000000000000000),
 ( 1.000000000000000000, 0.7203159680551509680, 1.000000000000000000),
 ( 1.000000000000000000, 0.7202477793832563480, 1.000000000000000000) ) ) 
 REPRESENTATION_ITEM ( '' )  SURFACE ( )  );
#4998 = EDGE_CURVE ( 'NONE', #5939, #13046, #17792, .T. ) ;
#4999 = DIRECTION ( 'NONE',  ( 0.9909299940865187173, -0.1338359446631173233, -0.01207007604876291287 ) ) ;
#5000 = CARTESIAN_POINT ( 'NONE',  ( -146.5000000000000000, 18.00000000000000355, 10.00000000000001599 ) ) ;
#5001 = ORIENTED_EDGE ( 'NONE', *, *, #16263, .F. ) ;
#5002 = CARTESIAN_POINT ( 'NONE',  ( 12.52469039290287611, 187.5804275016522240, 322.9582397512710941 ) ) ;
#5003 = ORIENTED_EDGE ( 'NONE', *, *, #6709, .T. ) ;
#5004 = CARTESIAN_POINT ( 'NONE',  ( 3.316624388958365088, 166.4147108432491109, 256.6009726804241495 ) ) ;
#5005 = CARTESIAN_POINT ( 'NONE',  ( 106.7514472241618790, 78.38843585434908334, -26.63023763040614966 ) ) ;
#5006 = DIRECTION ( 'NONE',  ( 0.9934404589540153374, 0.1135548637187135251, -0.01346653032743037014 ) ) ;
#5007 = EDGE_CURVE ( 'NONE', #1264, #1183, #20129, .T. ) ;
#5008 = ORIENTED_EDGE ( 'NONE', *, *, #12494, .F. ) ;
#5009 = CARTESIAN_POINT ( 'NONE',  ( 161.9999999999992610, 2.000000000000000000, -53.76161406891482386 ) ) ;
#5010 = VERTEX_POINT ( 'NONE', #308 ) ;
#5011 = ADVANCED_FACE ( 'NONE', ( #7298 ), #6957, .T. ) ;
#5012 = LINE ( 'NONE', #8798, #20530 ) ;
#5013 = CARTESIAN_POINT ( 'NONE',  ( -164.0000000000000000, 1.999999999999998224, -53.76161406891256433 ) ) ;
#5014 = CARTESIAN_POINT ( 'NONE',  ( -42.54575983488186353, 169.7656965055118974, -41.95299061980001198 ) ) ;
#5015 = CARTESIAN_POINT ( 'NONE',  ( 16.38239381841655984, 185.4577457402829168, 306.4392643500532927 ) ) ;
#5016 = CARTESIAN_POINT ( 'NONE',  ( -15.84248910266482646, 175.4932347526660692, 89.66429445754454264 ) ) ;
#5017 = DIRECTION ( 'NONE',  ( 0.9726991065672923042, 0.2316562896908778701, -0.01384960395994898341 ) ) ;
#5018 = CIRCLE ( 'NONE', #20060, 5.699999999999990408 ) ;
#5019 = PLANE ( 'NONE',  #3478 ) ;
#5020 = EDGE_CURVE ( 'NONE', #7715, #5612, #18454, .T. ) ;
#5021 = CONTEXT_DEPENDENT_SHAPE_REPRESENTATION ( #19672, #18713 ) ;
#5023 = ORIENTED_EDGE ( 'NONE', *, *, #2460, .F. ) ;
#5022 = ORIENTED_EDGE ( 'NONE', *, *, #9061, .F. ) ;
#5024 = LINE ( 'NONE', #19276, #839 ) ;
#5025 = DIRECTION ( 'NONE',  ( 0.01292394549866738782, 0.005513023399720700692, 0.9999012842304693116 ) ) ;
#5026 = LINE ( 'NONE', #12057, #3678 ) ;
#5027 = CARTESIAN_POINT ( 'NONE',  ( -10.81071488200823083, 114.1241249066815442, 131.6527946368535709 ) ) ;
#5028 = ORIENTED_EDGE ( 'NONE', *, *, #3184, .T. ) ;
#5029 = DIRECTION ( 'NONE',  ( 0.01125613334114018010, 0.4913919529878011949, 0.8708658036695671179 ) ) ;
#5030 = CARTESIAN_POINT ( 'NONE',  ( -51.39797222600954996, 113.2588685554743790, -43.52721704555492011 ) ) ;
#5031 = ORIENTED_EDGE ( 'NONE', *, *, #13304, .F. ) ;
#5032 = CARTESIAN_POINT ( 'NONE',  ( 48.26683418982636908, 111.5078795592862662, -44.80575254011499453 ) ) ;
#5033 = VERTEX_POINT ( 'NONE', #18231 ) ;
#5034 =( NAMED_UNIT ( * ) PLANE_ANGLE_UNIT ( ) SI_UNIT ( $, .RADIAN. ) );
#5035 = CARTESIAN_POINT ( 'NONE',  ( 106.8361484267443871, 79.08880628745905028, 26.19276530885263199 ) ) ;
#5036 = FACE_OUTER_BOUND ( 'NONE', #1616, .T. ) ;
#5037 = DIRECTION ( 'NONE',  ( -5.440186201345785633E-18, -1.000000000000000000, -1.334940939666367878E-17 ) ) ;
#5038 = AXIS2_PLACEMENT_3D ( 'NONE', #7120, #15646, #12651 ) ;
#5039 = ORIENTED_EDGE ( 'NONE', *, *, #22361, .F. ) ;
#5040 = EDGE_CURVE ( 'NONE', #11316, #8236, #8413, .T. ) ;
#5041 = CARTESIAN_POINT ( 'NONE',  ( -3.975234144917287438, 326.8809449508823946, 320.0352211315558293 ) ) ;
#5042 = DIRECTION ( 'NONE',  ( -0.9999164797902015955, 0.000000000000000000, 0.01292414190464162733 ) ) ;
#5043 = CIRCLE ( 'NONE', #17920, 83.00000000000004263 ) ;
#5044 = EDGE_CURVE ( 'NONE', #11676, #10601, #8045, .T. ) ;
#5045 = ORIENTED_EDGE ( 'NONE', *, *, #21469, .F. ) ;
#5046 = CARTESIAN_POINT ( 'NONE',  ( -53.01464514365870428, 126.5883500096206262, 107.5338433205492805 ) ) ;
#5047 = VERTEX_POINT ( 'NONE', #9481 ) ;
#5048 = AXIS2_PLACEMENT_3D ( 'NONE', #17307, #8557, #6511 ) ;
#5049 = LINE ( 'NONE', #10691, #14658 ) ;
#5050 = CARTESIAN_POINT ( 'NONE',  ( -88.16405828868519734, 88.32225945592601590, 52.86304920464149859 ) ) ;
#5051 = LINE ( 'NONE', #17374, #13739 ) ;
#5052 = ORIENTED_EDGE ( 'NONE', *, *, #4420, .T. ) ;
#5053 = ORIENTED_EDGE ( 'NONE', *, *, #15833, .T. ) ;
#5054 = DIRECTION ( 'NONE',  ( -0.4910069343201003411, 0.004767316193522951745, 0.8711426192914037969 ) ) ;
#5055 = CARTESIAN_POINT ( 'NONE',  ( 64.42259065992904254, 125.7553391191873544, -45.09312360222019578 ) ) ;
#5056 = CARTESIAN_POINT ( 'NONE',  ( -13.23978740117499164, 86.89928506224384819, -75.66871549674861797 ) ) ;
#5057 = DIRECTION ( 'NONE',  ( 0.000000000000000000, 0.000000000000000000, -1.000000000000000000 ) ) ;
#5058 = CARTESIAN_POINT ( 'NONE',  ( 104.8202145123290876, 69.99999999999998579, -33.35749735200946731 ) ) ;
#5059 = CARTESIAN_POINT ( 'NONE',  ( -52.93224801690938364, 189.4877715051681832, -92.28976992631349674 ) ) ;
#5060 = ORIENTED_EDGE ( 'NONE', *, *, #11604, .F. ) ;
#5061 = ORIENTED_EDGE ( 'NONE', *, *, #3904, .F. ) ;
#5062 = PLANE ( 'NONE',  #19502 ) ;
#5063 = DIRECTION ( 'NONE',  ( 7.125109674364536131E-05, -0.9999848031710253382, 0.005512562950849706628 ) ) ;
#5064 = CARTESIAN_POINT ( 'NONE',  ( 88.63197286364696481, 79.89291707602599502, -31.24418567530321766 ) ) ;
#5065 = DIRECTION ( 'NONE',  ( -0.01035335185279151644, -0.005513005182356664133, -0.9999312050732649393 ) ) ;
#5066 = AXIS2_PLACEMENT_3D ( 'NONE', #9910, #8510, #6571 ) ;
#5067 = CARTESIAN_POINT ( 'NONE',  ( -8.178437098313294129, 145.2910952780770515, 277.6650327932460414 ) ) ;
#5068 = VERTEX_POINT ( 'NONE', #11328 ) ;
#5069 = EDGE_CURVE ( 'NONE', #2773, #6559, #2562, .T. ) ;
#5070 = DIRECTION ( 'NONE',  ( 0.000000000000000000, 0.000000000000000000, 1.000000000000000000 ) ) ;
#5071 = CIRCLE ( 'NONE', #8012, 24.23418050574097293 ) ;
#5072 =( NAMED_UNIT ( * ) SI_UNIT ( $, .STERADIAN. ) SOLID_ANGLE_UNIT ( ) );
#5073 = AXIS2_PLACEMENT_3D ( 'NONE', #12203, #8612, #15888 ) ;
#5074 = CARTESIAN_POINT ( 'NONE',  ( -51.36859115140752152, 114.2028473779704143, 164.5977368973751993 ) ) ;
#5075 = CARTESIAN_POINT ( 'NONE',  ( 48.64240681911486774, 159.4614951111008452, 276.0554384422054000 ) ) ;
#5076 = EDGE_LOOP ( 'NONE', ( #10172, #6110, #1794, #4329 ) ) ;
#5077 = VERTEX_POINT ( 'NONE', #7543 ) ;
#5078 = UNCERTAINTY_MEASURE_WITH_UNIT (LENGTH_MEASURE( 1.000000000000000082E-05 ), #10154, 'distance_accuracy_value', 'NONE');
#5079 = B_SPLINE_CURVE_WITH_KNOTS ( 'NONE', 3,
 ( #4469, #13347, #22249, #9664, #18832, #16692, #9773, #7926, #20425, #6088, #13556, #17021, #6201, #16895, #13228 ),
 .UNSPECIFIED., .F., .F.,
 ( 4, 2, 1, 1, 1, 2, 2, 2, 4 ),
 ( -5.999999999001200712E-08, 3.336925554464112399E-05, 6.679851108927226935E-05, 0.0001336570221785711248, 0.0002673740443571829845, 0.0005348080887144481205, 0.001069676177429040734, 0.002139412354858207313, 0.004278884709716497536 ),
 .UNSPECIFIED. ) ;
#5080 = CARTESIAN_POINT ( 'NONE',  ( -90.00000000000000000, 29.00000000000000355, -10.99999999999999289 ) ) ;
#5081 = ORIENTED_EDGE ( 'NONE', *, *, #3620, .T. ) ;
#5082 = PRODUCT_RELATED_PRODUCT_CATEGORY ( 'part', '', ( #18549 ) ) ;
#5083 = DIRECTION ( 'NONE',  ( -0.9998688410312766006, -0.009690170827377751067, 0.01297695357578096571 ) ) ;
#5084 = AXIS2_PLACEMENT_3D ( 'NONE', #13341, #4574, #11834 ) ;
#5085 = DIRECTION ( 'NONE',  ( 0.000000000000000000, 0.000000000000000000, -1.000000000000000000 ) ) ;
#5086 = CARTESIAN_POINT ( 'NONE',  ( -91.62437796271721879, 72.00000000000000000, -60.86849236629028326 ) ) ;
#5087 = CARTESIAN_POINT ( 'NONE',  ( -49.64992578782946708, 140.1470953820375200, 27.40769847641930212 ) ) ;
#5088 = FACE_OUTER_BOUND ( 'NONE', #21676, .T. ) ;
#5089 = CARTESIAN_POINT ( 'NONE',  ( -12.64688860274155324, 109.6831087301383860, 124.2482791415423691 ) ) ;
#5090 = CARTESIAN_POINT ( 'NONE',  ( -56.96084827672684980, 114.2356707588182019, 162.8074586289424985 ) ) ;
#5091 = VERTEX_POINT ( 'NONE', #651 ) ;
#5092 = CLOSED_SHELL ( 'NONE', ( #1746, #17472, #18324, #6441, #13368, #11498, #22573, #8654, #20135, #22494, #12152, #407, #7804, #3647, #18948, #18979, #926, #12593, #12623, #2353 ) ) ;
#5093 = AXIS2_PLACEMENT_3D ( 'NONE', #14340, #21311, #9372 ) ;
#5094 = EDGE_CURVE ( 'NONE', #13282, #10108, #9137, .T. ) ;
#5095 = DIRECTION ( 'NONE',  ( -7.125109674161230605E-05, 0.9999848031710253382, -0.005512562950850140309 ) ) ;
#5096 = CARTESIAN_POINT ( 'NONE',  ( -11.19153202869804353, 137.5572120012638777, 101.3144779797563189 ) ) ;
#5097 = CIRCLE ( 'NONE', #18684, 2.000000000000004885 ) ;
#5098 = ORIENTED_EDGE ( 'NONE', *, *, #11887, .T. ) ;
#5099 = DIRECTION ( 'NONE',  ( 0.9999164797902015955, 2.001050586450178695E-22, -0.01292414190464131335 ) ) ;
#5100 = ORIENTED_EDGE ( 'NONE', *, *, #19412, .T. ) ;
#5101 = DIRECTION ( 'NONE',  ( 0.000000000000000000, 1.000000000000000000, 0.000000000000000000 ) ) ;
#5102 = EDGE_CURVE ( 'NONE', #4475, #440, #14303, .T. ) ;
#5103 = AXIS2_PLACEMENT_3D ( 'NONE', #3987, #2287, #1140 ) ;
#5104 = DIRECTION ( 'NONE',  ( 0.01292394549866731669, 0.005513023399720593139, 0.9999012842304692006 ) ) ;
#5105 =( GEOMETRIC_REPRESENTATION_CONTEXT ( 3 ) GLOBAL_UNCERTAINTY_ASSIGNED_CONTEXT ( ( #4235 ) ) GLOBAL_UNIT_ASSIGNED_CONTEXT ( ( #18564, #13513, #2823 ) ) REPRESENTATION_CONTEXT ( 'NONE', 'WORKASPACE' ) );
#5106 = CARTESIAN_POINT ( 'NONE',  ( -104.9795361740883521, 70.06102247219405399, 32.85291587203226271 ) ) ;
#5107 = CARTESIAN_POINT ( 'NONE',  ( 14.28940378674282208, 144.6940418464262166, 276.8225175484434999 ) ) ;
#5108 = EDGE_CURVE ( 'NONE', #21164, #20198, #21235, .T. ) ;
#5109 = EDGE_LOOP ( 'NONE', ( #3059, #14642, #22576, #2405 ) ) ;
#5110 = AXIS2_PLACEMENT_3D ( 'NONE', #11239, #17916, #2152 ) ;
#5111 = CARTESIAN_POINT ( 'NONE',  ( 16.40873467034997191, 185.6567299720572350, 322.3321779654821171 ) ) ;
#5112 = EDGE_LOOP ( 'NONE', ( #5374, #7654, #17754, #8951 ) ) ;
#5113 = ORIENTED_EDGE ( 'NONE', *, *, #7992, .T. ) ;
#5114 = CARTESIAN_POINT ( 'NONE',  ( -11.23547344339351284, 137.5384677217048193, 97.91481361337272915 ) ) ;
#5115 = CARTESIAN_POINT ( 'NONE',  ( 107.3521087218812369, 77.72700746170281150, -24.01651628897757007 ) ) ;
#5116 = CARTESIAN_POINT ( 'NONE',  ( -41.52238611146507452, 166.0448094368137504, 269.1837510020998820 ) ) ;
#5117 = VECTOR ( 'NONE', #19830, 1000.000000000000000 ) ;
#5118 = DIRECTION ( 'NONE',  ( 0.000000000000000000, 0.000000000000000000, 1.000000000000000000 ) ) ;
#5119 = ORIENTED_EDGE ( 'NONE', *, *, #14300, .F. ) ;
#5120 = EDGE_CURVE ( 'NONE', #5033, #17368, #10950, .T. ) ;
#5121 = DIRECTION ( 'NONE',  ( 7.125109674364534776E-05, -0.9999848031710252272, 0.005512562950849704893 ) ) ;
#5122 = EDGE_CURVE ( 'NONE', #2491, #20773, #21751, .T. ) ;
#5123 = DIRECTION ( 'NONE',  ( -0.01292394549866741557, -0.005513023399720270480, -0.9999012842304693116 ) ) ;
#5124 = DIRECTION ( 'NONE',  ( -0.01035335185279127358, -0.005513005182357338940, -0.9999312050732649393 ) ) ;
#5125 = CYLINDRICAL_SURFACE ( 'NONE', #20542, 2.000000000000001332 ) ;
#5126 = AXIS2_PLACEMENT_3D ( 'NONE', #17087, #20615, #8230 ) ;
#5127 = STYLED_ITEM ( 'NONE', ( #19343 ), #17564 ) ;
#5128 = FACE_OUTER_BOUND ( 'NONE', #19466, .T. ) ;
#5129 =( BOUNDED_CURVE ( )  B_SPLINE_CURVE ( 3, ( #7292, #14331, #7533, #5785 ),
 .UNSPECIFIED., .F., .T. ) 
 B_SPLINE_CURVE_WITH_KNOTS ( ( 4, 4 ),
 ( 5.799006443144740786, 5.835910511159155156 ),
 .UNSPECIFIED. ) 
 CURVE ( )  GEOMETRIC_REPRESENTATION_ITEM ( )  RATIONAL_B_SPLINE_CURVE ( ( 1.000000000000000000, 0.9998865107004336616, 0.9998865107004336616, 1.000000000000000000 ) ) 
 REPRESENTATION_ITEM ( '' )  );
#5130 = CARTESIAN_POINT ( 'NONE',  ( 33.82085273160093664, 93.50464841319750064, -82.93470554904388337 ) ) ;
#5131 = EDGE_LOOP ( 'NONE', ( #15559, #18865, #15546, #21097 ) ) ;
#5132 = EDGE_LOOP ( 'NONE', ( #12174, #17019, #6661, #19560, #16084, #19536, #15385, #491, #18766, #6770, #14536 ) ) ;
#5133 = DIRECTION ( 'NONE',  ( 0.01292414190464177652, 1.902755938799532355E-22, 0.9999164797902015955 ) ) ;
#5134 = DIRECTION ( 'NONE',  ( -0.9726991065672923042, -0.2316562896908775926, 0.01384960395994898341 ) ) ;
#5135 = ADVANCED_FACE ( 'NONE', ( #18326 ), #22172, .F. ) ;
#5136 = VECTOR ( 'NONE', #14814, 1000.000000000000114 ) ;
#5137 = ORIENTED_EDGE ( 'NONE', *, *, #2763, .T. ) ;
#5138 = CARTESIAN_POINT ( 'NONE',  ( -50.59335657864021840, 108.5738102592509335, -45.58376217401134056 ) ) ;
#5139 = EDGE_CURVE ( 'NONE', #7464, #9403, #18680, .T. ) ;
#5140 = DIRECTION ( 'NONE',  ( -0.01292394549866727679, -0.005513023399720743192, -0.9999012842304693116 ) ) ;
#5141 = DIRECTION ( 'NONE',  ( 0.009760756503427210282, -0.9999378516499566327, 0.005387065077606872227 ) ) ;
#5142 = AXIS2_PLACEMENT_3D ( 'NONE', #10381, #7256, #2096 ) ;
#5143 = ORIENTED_EDGE ( 'NONE', *, *, #15467, .T. ) ;
#5144 = CARTESIAN_POINT ( 'NONE',  ( 90.40889375659912730, 69.99999999999998579, -33.17122784026042837 ) ) ;
#5145 = PRODUCT_DEFINITION_SHAPE ( 'NONE', 'NONE',  #22695 ) ;
#5146 = DIRECTION ( 'NONE',  ( 0.009188991635466048358, -0.7031977391749438810, 0.7109349492407661675 ) ) ;
#5147 = VERTEX_POINT ( 'NONE', #17611 ) ;
#5148 = FACE_OUTER_BOUND ( 'NONE', #5647, .T. ) ;
#5149 = ORIENTED_EDGE ( 'NONE', *, *, #2216, .F. ) ;
#5150 = TOROIDAL_SURFACE ( 'NONE', #3325, 8.000000000000014211, 2.000000000000000000 ) ;
#5151 = CARTESIAN_POINT ( 'NONE',  ( 106.4939345422100985, 78.92840590577354476, 27.55192737125488023 ) ) ;
#5152 = FACE_OUTER_BOUND ( 'NONE', #1166, .T. ) ;
#5153 = CARTESIAN_POINT ( 'NONE',  ( -41.56623493000980574, 91.17157287525390075, -82.46967996629571473 ) ) ;
#5154 = EDGE_CURVE ( 'NONE', #20401, #14389, #2173, .T. ) ;
#5155 = DIRECTION ( 'NONE',  ( -0.01292394549866632963, -0.005513023399716958026, -0.9999012842304692006 ) ) ;
#5156 =( LENGTH_UNIT ( ) NAMED_UNIT ( * ) SI_UNIT ( .MILLI., .METRE. ) );
#5157 = VERTEX_POINT ( 'NONE', #11906 ) ;
#5158 = CARTESIAN_POINT ( 'NONE',  ( -1.405147466491028840, 327.1319313373589353, 309.3977247008179461 ) ) ;
#5159 = CARTESIAN_POINT ( 'NONE',  ( 13.18868299908003294, 189.1369543048038224, 275.2921301635565214 ) ) ;
#5160 = ORIENTED_EDGE ( 'NONE', *, *, #22642, .T. ) ;
#5161 = CARTESIAN_POINT ( 'NONE',  ( 90.02055463237803679, 71.90407553649232852, -63.21629334023821656 ) ) ;
#5162 = CIRCLE ( 'NONE', #18736, 3.399999999999991918 ) ;
#5163 = B_SPLINE_CURVE_WITH_KNOTS ( 'NONE', 3,
 ( #2989, #22160, #8170, #1297, #15530, #22261, #15420, #8485, #18842, #11726, #10008, #6551, #9888, #2877, #13361, #10230 ),
 .UNSPECIFIED., .F., .F.,
 ( 4, 2, 2, 2, 2, 2, 2, 4 ),
 ( 0.000000000000000000, 0.0003989315947993842177, 0.0007978631895987684354, 0.001196794784398152707, 0.001595726379197536871, 0.002393589568796304547, 0.002792521163595683073, 0.003191452758395061599 ),
 .UNSPECIFIED. ) ;
#5164 = CARTESIAN_POINT ( 'NONE',  ( -89.53501783834650496, 89.09639617097565178, 51.70581852932981803 ) ) ;
#5165 = DIRECTION ( 'NONE',  ( 0.9934404589540163366, 0.1135548637187057258, -0.01346653032743021922 ) ) ;
#5166 = AXIS2_PLACEMENT_3D ( 'NONE', #18975, #10258, #10380 ) ;
#5167 = EDGE_LOOP ( 'NONE', ( #10414, #4621, #6636 ) ) ;
#5168 = EDGE_CURVE ( 'NONE', #8739, #9852, #17292, .T. ) ;
#5169 = EDGE_LOOP ( 'NONE', ( #12023, #15573, #11662, #7611, #21887 ) ) ;
#5170 = CARTESIAN_POINT ( 'NONE',  ( -73.39659566742001573, 95.91349339596638401, 81.93264795988667970 ) ) ;
#5171 = AXIS2_PLACEMENT_3D ( 'NONE', #7648, #391, #3837 ) ;
#5172 = CARTESIAN_POINT ( 'NONE',  ( 45.33978850604763977, 173.1465938866814156, 25.99799041810029010 ) ) ;
#5173 = FILL_AREA_STYLE_COLOUR ( '', #7318 ) ;
#5174 = CARTESIAN_POINT ( 'NONE',  ( 84.00592537107472424, 75.05062594699531076, -4.199599686265332643 ) ) ;
#5175 = PLANE ( 'NONE',  #18835 ) ;
#5176 = ORIENTED_EDGE ( 'NONE', *, *, #4888, .T. ) ;
#5177 = ORIENTED_EDGE ( 'NONE', *, *, #1346, .T. ) ;
#5178 = CARTESIAN_POINT ( 'NONE',  ( -13.50073983619024176, 183.7065926015648074, 278.6553669534396249 ) ) ;
#5179 = CARTESIAN_POINT ( 'NONE',  ( -65.56436017564475094, 94.99786382055523859, -43.24343005912400173 ) ) ;
#5180 = LINE ( 'NONE', #14282, #18967 ) ;
#5181 = CARTESIAN_POINT ( 'NONE',  ( -23.62788402525385578, 324.6350553711861835, 320.4254447255032119 ) ) ;
#5182 = AXIS2_PLACEMENT_3D ( 'NONE', #3787, #10810, #15878 ) ;
#5183 = CIRCLE ( 'NONE', #4448, 8.000000000000014211 ) ;
#5184 = DIRECTION ( 'NONE',  ( 5.440186201345738641E-18, 1.000000000000000000, 1.334940939666364181E-17 ) ) ;
#5185 = EDGE_CURVE ( 'NONE', #11619, #5755, #10984, .T. ) ;
#5186 = EDGE_LOOP ( 'NONE', ( #15307, #16621, #12909, #13205, #12894, #11757, #12518, #2587, #6055, #8761, #2462, #21349, #19656, #6379, #13919, #17760, #2891, #1048, #9357, #1175, #21767, #9151, #21144, #12115, #6958, #12185, #2395, #3886, #20657, #11933, #22332, #4316, #19658, #8375, #17898, #7556, #12749, #20871 ) ) ;
#5187 = FACE_OUTER_BOUND ( 'NONE', #1385, .T. ) ;
#5188 = CIRCLE ( 'NONE', #8867, 22.50000000000000355 ) ;
#5189 = DIRECTION ( 'NONE',  ( -7.125109674118361251E-05, 0.9999848031710253382, -0.005512562950849477644 ) ) ;
#5190 = ORIENTED_EDGE ( 'NONE', *, *, #3011, .F. ) ;
#5191 = CIRCLE ( 'NONE', #827, 2.000000000000001776 ) ;
#5192 = FACE_OUTER_BOUND ( 'NONE', #8383, .T. ) ;
#5193 = ORIENTED_EDGE ( 'NONE', *, *, #5577, .F. ) ;
#5194 = ORIENTED_EDGE ( 'NONE', *, *, #12186, .T. ) ;
#5195 = EDGE_LOOP ( 'NONE', ( #6515, #7457, #20834, #19894 ) ) ;
#5196 = CARTESIAN_POINT ( 'NONE',  ( 19.33710169866840189, 184.3365238270897066, 311.8886436260900723 ) ) ;
#5197 = CIRCLE ( 'NONE', #3393, 7.999999999999985789 ) ;
#5199 = ORIENTED_EDGE ( 'NONE', *, *, #12045, .T. ) ;
#5198 = ORIENTED_EDGE ( 'NONE', *, *, #13085, .F. ) ;
#5200 = VECTOR ( 'NONE', #3538, 999.9999999999998863 ) ;
#5201 = MECHANICAL_DESIGN_GEOMETRIC_PRESENTATION_REPRESENTATION (  '', ( #5933 ), #6321 ) ;
#5202 = ADVANCED_FACE ( 'NONE', ( #17176 ), #9943, .F. ) ;
#5203 = CARTESIAN_POINT ( 'NONE',  ( 44.62344841673417761, 166.7281037598372961, 233.8131482778615293 ) ) ;
#5204 = CARTESIAN_POINT ( 'NONE',  ( 92.14659905926313854, 77.13858430795839638, -31.20924108170689593 ) ) ;
#5205 = EDGE_CURVE ( 'NONE', #13022, #16435, #6589, .T. ) ;
#5206 = PLANE ( 'NONE',  #19572 ) ;
#5207 = LINE ( 'NONE', #10737, #1267 ) ;
#5208 = VECTOR ( 'NONE', #16897, 1000.000000000000114 ) ;
#5209 = DIRECTION ( 'NONE',  ( -0.9909299940865188283, 0.1338359446631173788, 0.01207007604876290420 ) ) ;
#5210 = CARTESIAN_POINT ( 'NONE',  ( 0.000000000000000000, 1.999999999999998224, 0.000000000000000000 ) ) ;
#5211 = CARTESIAN_POINT ( 'NONE',  ( 12.02049240483441750, 187.6813724364916425, 304.8898053572733602 ) ) ;
#5212 = CARTESIAN_POINT ( 'NONE',  ( -52.39628412465351914, 189.6008764489689611, -71.77933984920133526 ) ) ;
#5213 = CARTESIAN_POINT ( 'NONE',  ( 92.64101326278361626, 79.05197601643139649, 26.25411123107249267 ) ) ;
#5214 = VECTOR ( 'NONE', #1869, 1000.000000000000114 ) ;
#5215 = CARTESIAN_POINT ( 'NONE',  ( -64.64767546932813502, 126.1473081376430798, 27.67873648630093797 ) ) ;
#5216 = ORIENTED_EDGE ( 'NONE', *, *, #10833, .T. ) ;
#5217 = CARTESIAN_POINT ( 'NONE',  ( -91.45164190239951552, 80.14421549785515708, -29.66212192225370359 ) ) ;
#5218 = EDGE_LOOP ( 'NONE', ( #13370, #671, #21765, #18069 ) ) ;
#5219 = EDGE_CURVE ( 'NONE', #5976, #11327, #12335, .T. ) ;
#5220 = LINE ( 'NONE', #12260, #15884 ) ;
#5221 = FACE_OUTER_BOUND ( 'NONE', #10958, .T. ) ;
#5222 = CIRCLE ( 'NONE', #4496, 4.199999999999997513 ) ;
#5223 = AXIS2_PLACEMENT_3D ( 'NONE', #18844, #10126, #6458 ) ;
#5224 = CARTESIAN_POINT ( 'NONE',  ( -9.472248412593200939, 69.99999999999998579, -86.53426659026914081 ) ) ;
#5225 = DIRECTION ( 'NONE',  ( 7.125109674160258889E-05, -0.9999848031710253382, 0.005512562950849898315 ) ) ;
#5226 = LINE ( 'NONE', #10979, #11502 ) ;
#5227 = ORIENTED_EDGE ( 'NONE', *, *, #19350, .T. ) ;
#5228 = CARTESIAN_POINT ( 'NONE',  ( 13.12964460975451608, 190.2538275423460163, 320.8426553563187440 ) ) ;
#5229 = VERTEX_POINT ( 'NONE', #8426 ) ;
#5230 = LINE ( 'NONE', #4474, #8939 ) ;
#5231 = CARTESIAN_POINT ( 'NONE',  ( 93.23587179807657321, 72.00000000000000000, 30.79757858250317071 ) ) ;
#5232 = CARTESIAN_POINT ( 'NONE',  ( -11.02481633791520998, 186.5310056599434176, 320.9512889225665049 ) ) ;
#5233 = ADVANCED_BREP_SHAPE_REPRESENTATION ( '', ( #9541, #6292 ), #13288 ) ;
#5234 = DIRECTION ( 'NONE',  ( -0.01292394549866750231, -0.005513023399722823126, -0.9999012842304692006 ) ) ;
#5235 = AXIS2_PLACEMENT_3D ( 'NONE', #16975, #18890, #4644 ) ;
#5236 = VERTEX_POINT ( 'NONE', #22428 ) ;
#5237 = CARTESIAN_POINT ( 'NONE',  ( 40.63089462960166287, 93.08398165842314143, 83.39786430079456636 ) ) ;
#5238 = CARTESIAN_POINT ( 'NONE',  ( -90.77986998051284218, 77.66088650200015309, 32.02971036561880425 ) ) ;
#5239 = DIRECTION ( 'NONE',  ( 0.9999164797902017066, 2.001050586450178931E-22, -0.01292414190464131508 ) ) ;
#5240 = DIRECTION ( 'NONE',  ( 0.000000000000000000, 0.000000000000000000, 1.000000000000000000 ) ) ;
#5241 = VECTOR ( 'NONE', #9729, 999.9999999999998863 ) ;
#5242 = CIRCLE ( 'NONE', #1254, 8.000000000000003553 ) ;
#5243 = CARTESIAN_POINT ( 'NONE',  ( 19.98044029014978307, 182.5758476881784702, 310.8270597400842234 ) ) ;
#5244 = CARTESIAN_POINT ( 'NONE',  ( 67.23320572660466610, 192.1022009597330680, 17.60971032628828681 ) ) ;
#5245 = ORIENTED_EDGE ( 'NONE', *, *, #2229, .T. ) ;
#5246 = LINE ( 'NONE', #20994, #21592 ) ;
#5247 = DIRECTION ( 'NONE',  ( -0.01292394549866632963, -0.005513023399716958026, -0.9999012842304692006 ) ) ;
#5248 = CONTEXT_DEPENDENT_SHAPE_REPRESENTATION ( #11926, #3513 ) ;
#5249 = AXIS2_PLACEMENT_3D ( 'NONE', #18516, #15079, #20214 ) ;
#5250 = EDGE_CURVE ( 'NONE', #14111, #4461, #1860, .T. ) ;
#5251 = VERTEX_POINT ( 'NONE', #256 ) ;
#5252 = ADVANCED_FACE ( 'NONE', ( #16463 ), #5744, .T. ) ;
#5253 = DIRECTION ( 'NONE',  ( -0.9999164797902015955, -6.965998958219364448E-18, 0.01292414190464157182 ) ) ;
#5254 = CARTESIAN_POINT ( 'NONE',  ( 1.364373935098378649E-14, 105.0000000000000000, -9.836450281572198869E-15 ) ) ;
#5255 = CARTESIAN_POINT ( 'NONE',  ( -16.82677409528017520, 137.4993252555668164, 90.88659727581192271 ) ) ;
#5256 = CYLINDRICAL_SURFACE ( 'NONE', #19163, 9.999999999999998224 ) ;
#5257 = CIRCLE ( 'NONE', #3065, 110.0000000000000000 ) ;
#5258 = ORIENTED_EDGE ( 'NONE', *, *, #15315, .F. ) ;
#5259 = DIRECTION ( 'NONE',  ( 0.000000000000000000, 0.000000000000000000, 1.000000000000000000 ) ) ;
#5260 = CONICAL_SURFACE ( 'NONE', #18147, 11.00000000000000178, 0.7853981633974346233 ) ;
#5261 = DIRECTION ( 'NONE',  ( 7.125109674364534776E-05, -0.9999848031710252272, 0.005512562950849704893 ) ) ;
#5262 = VERTEX_POINT ( 'NONE', #5985 ) ;
#5263 = CARTESIAN_POINT ( 'NONE',  ( 47.86827886238202723, 110.7146866689297582, -44.79622780157797735 ) ) ;
#5264 = ORIENTED_EDGE ( 'NONE', *, *, #8417, .T. ) ;
#5265 = CARTESIAN_POINT ( 'NONE',  ( -1.163172771417702700, 37.00000000000000711, -89.99248318111824574 ) ) ;
#5266 = CARTESIAN_POINT ( 'NONE',  ( 54.52327687265659506, 1.999999999999998224, 111.3697098814018744 ) ) ;
#5267 = CARTESIAN_POINT ( 'NONE',  ( 48.84321673125851504, 168.6907664596096765, 33.97806514274709144 ) ) ;
#5268 = FACE_OUTER_BOUND ( 'NONE', #5437, .T. ) ;
#5269 = EDGE_CURVE ( 'NONE', #22319, #5077, #484, .T. ) ;
#5270 = ORIENTED_EDGE ( 'NONE', *, *, #672, .F. ) ;
#5271 = CARTESIAN_POINT ( 'NONE',  ( -48.80449223365644684, 105.5072037373731888, 92.81729778463858338 ) ) ;
#5272 = DIRECTION ( 'NONE',  ( 0.000000000000000000, 0.000000000000000000, -1.000000000000000000 ) ) ;
#5273 = VECTOR ( 'NONE', #341, 999.9999999999998863 ) ;
#5274 = ORIENTED_EDGE ( 'NONE', *, *, #17991, .F. ) ;
#5275 = CARTESIAN_POINT ( 'NONE',  ( -1.291844632700186013, 327.1802634178375797, 318.1637512231440041 ) ) ;
#5276 = EDGE_CURVE ( 'NONE', #17777, #22622, #3810, .T. ) ;
#5277 = DIRECTION ( 'NONE',  ( 0.01246513159389404414, 0.2641402835564772844, 0.9644037178988117409 ) ) ;
#5278 = ORIENTED_EDGE ( 'NONE', *, *, #14712, .F. ) ;
#5279 = AXIS2_PLACEMENT_3D ( 'NONE', #310, #12829, #14465 ) ;
#5280 = AXIS2_PLACEMENT_3D ( 'NONE', #1595, #8463, #12046 ) ;
#5281 = CYLINDRICAL_SURFACE ( 'NONE', #20486, 6.000000000000000888 ) ;
#5282 = CARTESIAN_POINT ( 'NONE',  ( -88.16582745102967067, 88.48269947768268651, 52.70639469617027117 ) ) ;
#5283 = B_SPLINE_CURVE_WITH_KNOTS ( 'NONE', 3,
 ( #19115, #1897, #5772, #14440, #7279, #2226 ),
 .UNSPECIFIED., .F., .F.,
 ( 4, 2, 4 ),
 ( 0.000000000000000000, 0.0009922935535326162220, 0.001984587107065232444 ),
 .UNSPECIFIED. ) ;
#5284 = VERTEX_POINT ( 'NONE', #12895 ) ;
#5285 = ADVANCED_FACE ( 'NONE', ( #19749 ), #11046, .T. ) ;
#5286 = EDGE_LOOP ( 'NONE', ( #9687, #15268, #13597, #17306 ) ) ;
#5287 = DIRECTION ( 'NONE',  ( -0.000000000000000000, -1.000000000000000000, -0.000000000000000000 ) ) ;
#5288 = CARTESIAN_POINT ( 'NONE',  ( -13.51080300167352810, 109.6914967035374673, 125.7810327540168629 ) ) ;
#5289 = AXIS2_PLACEMENT_3D ( 'NONE', #9894, #18728, #21813 ) ;
#5290 = DIRECTION ( 'NONE',  ( -0.9934404589540172248, -0.1135548637186977322, 0.01346653032743275885 ) ) ;
#5291 = ADVANCED_FACE ( 'NONE', ( #14278 ), #14684, .T. ) ;
#5292 = DIRECTION ( 'NONE',  ( 0.9999164797902015955, 6.965998958219364448E-18, -0.01292414190464157182 ) ) ;
#5293 = DIRECTION ( 'NONE',  ( -0.000000000000000000, -1.000000000000000000, -0.000000000000000000 ) ) ;
#5294 = EDGE_LOOP ( 'NONE', ( #8723, #16544 ) ) ;
#5295 = DIRECTION ( 'NONE',  ( -7.125109674243555432E-05, 0.9999848031710253382, -0.005512562950850175003 ) ) ;
#5296 = VERTEX_POINT ( 'NONE', #7485 ) ;
#5297 = DIRECTION ( 'NONE',  ( -7.125109674243555432E-05, 0.9999848031710253382, -0.005512562950850175003 ) ) ;
#5298 = CARTESIAN_POINT ( 'NONE',  ( -75.13217090412312871, 75.01367125662450519, 2.612192813631355914 ) ) ;
#5299 = CARTESIAN_POINT ( 'NONE',  ( -22.40767239932358379, 324.7751959534260777, 320.5736243973683486 ) ) ;
#5300 = AXIS2_PLACEMENT_3D ( 'NONE', #2758, #9767, #15295 ) ;
#5301 = LINE ( 'NONE', #373, #22006 ) ;
#5302 = ORIENTED_EDGE ( 'NONE', *, *, #18906, .T. ) ;
#5303 = CARTESIAN_POINT ( 'NONE',  ( -1.163172771417702700, 81.99999999999998579, -89.99248318111824574 ) ) ;
#5304 = DIRECTION ( 'NONE',  ( -0.004263634442766563518, -0.9440169652124856814, -0.3298693541575922761 ) ) ;
#5305 = DIRECTION ( 'NONE',  ( 0.009760756503428011724, -0.9999378516499566327, 0.005387065077610982654 ) ) ;
#5306 = VERTEX_POINT ( 'NONE', #3684 ) ;
#5307 = ADVANCED_FACE ( 'NONE', ( #5864 ), #17606, .F. ) ;
#5308 = LINE ( 'NONE', #12348, #7014 ) ;
#5309 = ORIENTED_EDGE ( 'NONE', *, *, #18645, .T. ) ;
#5310 = AXIS2_PLACEMENT_3D ( 'NONE', #2675, #1056, #8047 ) ;
#5311 = ORIENTED_EDGE ( 'NONE', *, *, #4149, .F. ) ;
#5312 = ORIENTED_EDGE ( 'NONE', *, *, #3449, .T. ) ;
#5313 = UNCERTAINTY_MEASURE_WITH_UNIT (LENGTH_MEASURE( 1.000000000000000082E-05 ), #15714, 'distance_accuracy_value', 'NONE');
#5314 = CARTESIAN_POINT ( 'NONE',  ( 19.91562502177398386, 183.5286201153226386, 313.8266703284822938 ) ) ;
#5315 = EDGE_LOOP ( 'NONE', ( #2364, #11460 ) ) ;
#5316 = EDGE_CURVE ( 'NONE', #5956, #20235, #15108, .T. ) ;
#5317 = CARTESIAN_POINT ( 'NONE',  ( 19.99832959580401948, 170.0000000000008242, -0.2584828380919867996 ) ) ;
#5318 = CARTESIAN_POINT ( 'NONE',  ( 51.07356891511743413, 94.48610424851698042, 82.73688480180348392 ) ) ;
#5319 = DIRECTION ( 'NONE',  ( -0.01292394549866632963, -0.005513023399716958026, -0.9999012842304692006 ) ) ;
#5320 = DIRECTION ( 'NONE',  ( 7.125109674364534776E-05, -0.9999848031710252272, 0.005512562950849704893 ) ) ;
#5321 = PLANE ( 'NONE',  #13171 ) ;
#5322 = CARTESIAN_POINT ( 'NONE',  ( -40.91700983470048669, 95.59801226234188221, 82.80155338050317937 ) ) ;
#5323 = AXIS2_PLACEMENT_3D ( 'NONE', #12075, #15536, #13907 ) ;
#5324 = CARTESIAN_POINT ( 'NONE',  ( 82.68550139462496418, 75.16567244870638831, -6.678086237966566863 ) ) ;
#5325 = CARTESIAN_POINT ( 'NONE',  ( 11.99112089040652762, 187.7242859511004838, 307.7456636232291203 ) ) ;
#5326 = CARTESIAN_POINT ( 'NONE',  ( 92.55117574443833917, 77.19412514573775752, 28.91372802644201911 ) ) ;
#5327 = CARTESIAN_POINT ( 'NONE',  ( -84.36252974213540767, 104.9530375760216856, -70.59083440939244269 ) ) ;
#5328 = ORIENTED_EDGE ( 'NONE', *, *, #3442, .F. ) ;
#5329 =( LENGTH_UNIT ( ) NAMED_UNIT ( * ) SI_UNIT ( .MILLI., .METRE. ) );
#5330 = EDGE_CURVE ( 'NONE', #11842, #1325, #4137, .T. ) ;
#5331 = FACE_OUTER_BOUND ( 'NONE', #6608, .T. ) ;
#5332 = DIRECTION ( 'NONE',  ( -0.01035335185279143318, -0.005513005182356926943, -0.9999312050732649393 ) ) ;
#5333 = ADVANCED_FACE ( 'NONE', ( #14405 ), #18182, .F. ) ;
#5334 = VERTEX_POINT ( 'NONE', #7706 ) ;
#5335 = CARTESIAN_POINT ( 'NONE',  ( -91.97397837737942439, 77.39048292941923535, -29.24031187446860258 ) ) ;
#5336 = ORIENTED_EDGE ( 'NONE', *, *, #6130, .T. ) ;
#5337 = AXIS2_PLACEMENT_3D ( 'NONE', #5980, #16121, #19863 ) ;
#5338 = PRODUCT_DEFINITION_SHAPE ( 'NONE', 'NONE',  #22671 ) ;
#5339 = CARTESIAN_POINT ( 'NONE',  ( -64.07781825212431670, 106.8061942917681790, 71.76751443486088533 ) ) ;
#5340 = ORIENTED_EDGE ( 'NONE', *, *, #5568, .T. ) ;
#5341 = CARTESIAN_POINT ( 'NONE',  ( -45.67464185259402853, 168.2105890667581605, -51.90496219196452188 ) ) ;
#5342 = DIRECTION ( 'NONE',  ( -0.9726991065672923042, -0.2316562896908775926, 0.01384960395994898341 ) ) ;
#5343 = EDGE_LOOP ( 'NONE', ( #12524, #5537, #17319, #2208 ) ) ;
#5344 = FACE_OUTER_BOUND ( 'NONE', #11037, .T. ) ;
#5345 = ORIENTED_EDGE ( 'NONE', *, *, #406, .F. ) ;
#5346 = ORIENTED_EDGE ( 'NONE', *, *, #637, .T. ) ;
#5347 = DIRECTION ( 'NONE',  ( -0.01292394549866738608, -0.005513023399720468239, -0.9999012842304692006 ) ) ;
#5348 = CARTESIAN_POINT ( 'NONE',  ( 51.15216422151338804, 107.4645925609455901, 69.52715930618317941 ) ) ;
#5349 = FACE_OUTER_BOUND ( 'NONE', #10093, .T. ) ;
#5350 = DIRECTION ( 'NONE',  ( 0.6080604969667605664, 0.004419696743559108250, 0.7938783901261144971 ) ) ;
#5351 = CARTESIAN_POINT ( 'NONE',  ( -10.85595612533484911, 109.6999345499266525, 127.2773526115149281 ) ) ;
#5352 = ORIENTED_EDGE ( 'NONE', *, *, #612, .F. ) ;
#5353 = CARTESIAN_POINT ( 'NONE',  ( -13.60878576479588276, 182.9261561738083515, 319.2680663699061370 ) ) ;
#5354 = EDGE_CURVE ( 'NONE', #5504, #8741, #15422, .T. ) ;
#5355 = PRODUCT ( 'Stud', 'Stud', '', ( #15404 ) ) ;
#5356 = CARTESIAN_POINT ( 'NONE',  ( -51.42803251223699590, 189.3893605493459233, -110.1610646708163159 ) ) ;
#5357 = CARTESIAN_POINT ( 'NONE',  ( -14.05315427626016600, 180.0651354203414769, 318.4885795860537314 ) ) ;
#5358 = VERTEX_POINT ( 'NONE', #12675 ) ;
#5359 = CARTESIAN_POINT ( 'NONE',  ( 16.60281234097334746, 185.5290831433204062, 322.2010377526273146 ) ) ;
#5360 = CARTESIAN_POINT ( 'NONE',  ( -64.99457118636311748, 170.0000000000008242, 0.8400692238025471159 ) ) ;
#5361 = CARTESIAN_POINT ( 'NONE',  ( -5.156377330703347361, 70.80384757729338219, -99.58697729741749072 ) ) ;
#5362 = CARTESIAN_POINT ( 'NONE',  ( -11.14411950718743682, 81.44011527025983810, -90.55128027993727358 ) ) ;
#5363 = CARTESIAN_POINT ( 'NONE',  ( -33.79255210837673218, 93.51775827232349059, 82.92153020431163668 ) ) ;
#5364 = CARTESIAN_POINT ( 'NONE',  ( 24.56098209142228228, 169.1174711406635822, 324.3181961363840742 ) ) ;
#5365 = DIRECTION ( 'NONE',  ( 0.009760756503427111402, -0.9999378516499564107, 0.005387065077611765014 ) ) ;
#5366 = LINE ( 'NONE', #21221, #10660 ) ;
#5367 = FACE_OUTER_BOUND ( 'NONE', #9373, .T. ) ;
#5368 = VECTOR ( 'NONE', #8036, 1000.000000000000000 ) ;
#5369 = EDGE_LOOP ( 'NONE', ( #3226, #2651, #13058 ) ) ;
#5370 = DIRECTION ( 'NONE',  ( -0.000000000000000000, -1.000000000000000000, -0.000000000000000000 ) ) ;
#5371 = LINE ( 'NONE', #12410, #13963 ) ;
#5372 = VERTEX_POINT ( 'NONE', #17956 ) ;
#5373 = CARTESIAN_POINT ( 'NONE',  ( -106.2089377515398780, 77.12912189496638860, -28.62973177816246206 ) ) ;
#5374 = ORIENTED_EDGE ( 'NONE', *, *, #2751, .T. ) ;
#5375 = CARTESIAN_POINT ( 'NONE',  ( 9.914309459522627321, 174.9920644939733734, 324.4751176552225616 ) ) ;
#5376 = CARTESIAN_POINT ( 'NONE',  ( 1.054933926688728762, 165.4499317482979279, 81.61824794009152129 ) ) ;
#5377 = LINE ( 'NONE', #3662, #15862 ) ;
#5378 = DIRECTION ( 'NONE',  ( 0.000000000000000000, 0.000000000000000000, 1.000000000000000000 ) ) ;
#5379 = EDGE_CURVE ( 'NONE', #13946, #11196, #5753, .T. ) ;
#5380 = VECTOR ( 'NONE', #14711, 1000.000000000000000 ) ;
#5381 = CARTESIAN_POINT ( 'NONE',  ( 15.94290392677929269, 168.1183014920872267, 320.9451345667529836 ) ) ;
#5382 = DIRECTION ( 'NONE',  ( -0.9934404589540162256, -0.1135548637187056842, 0.01346653032743081423 ) ) ;
#5383 = ORIENTED_EDGE ( 'NONE', *, *, #6810, .F. ) ;
#5384 = FACE_OUTER_BOUND ( 'NONE', #10532, .T. ) ;
#5385 = CARTESIAN_POINT ( 'NONE',  ( -89.82946945839044872, 88.94369713871104466, 52.15294112658025938 ) ) ;
#5386 = ORIENTED_EDGE ( 'NONE', *, *, #13036, .T. ) ;
#5387 = EDGE_CURVE ( 'NONE', #8011, #7061, #2873, .T. ) ;
#5388 = ORIENTED_EDGE ( 'NONE', *, *, #669, .T. ) ;
#5389 = DIRECTION ( 'NONE',  ( -2.025474946048326158E-22, 1.000000000000000000, -1.876735158486679638E-22 ) ) ;
#5390 = ADVANCED_FACE ( 'NONE', ( #2543 ), #18515, .T. ) ;
#5391 = LINE ( 'NONE', #5635, #22427 ) ;
#5392 = CARTESIAN_POINT ( 'NONE',  ( 85.09728723043602372, 74.99999364505980282, -0.7689863871492244041 ) ) ;
#5393 = TOROIDAL_SURFACE ( 'NONE', #1399, 17.29295143883736330, 7.000000000000003553 ) ;
#5394 = DIRECTION ( 'NONE',  ( 7.125109674161447446E-05, -0.9999848031710253382, 0.005512562950850309444 ) ) ;
#5395 = ORIENTED_EDGE ( 'NONE', *, *, #881, .T. ) ;
#5396 = EDGE_CURVE ( 'NONE', #6708, #18167, #22154, .T. ) ;
#5397 = CARTESIAN_POINT ( 'NONE',  ( 17.25791503114635361, 186.5747366875307875, 277.7312368246228971 ) ) ;
#5398 = ORIENTED_EDGE ( 'NONE', *, *, #19604, .T. ) ;
#5399 = LINE ( 'NONE', #2321, #8444 ) ;
#5400 = AXIS2_PLACEMENT_3D ( 'NONE', #5254, #12299, #22355 ) ;
#5401 = PLANE ( 'NONE',  #22486 ) ;
#5402 = CARTESIAN_POINT ( 'NONE',  ( -74.91815584878337120, 75.00179123396262071, 1.637215763915028210 ) ) ;
#5403 = CARTESIAN_POINT ( 'NONE',  ( -12.21093709921540338, 164.8562217133218439, 310.4321100316089428 ) ) ;
#5404 = ORIENTED_EDGE ( 'NONE', *, *, #10803, .T. ) ;
#5405 = PLANE ( 'NONE',  #19093 ) ;
#5406 = ORIENTED_EDGE ( 'NONE', *, *, #17818, .F. ) ;
#5407 = CARTESIAN_POINT ( 'NONE',  ( -39.27191838138413260, 107.6444011096156999, 72.18501429557439053 ) ) ;
#5408 = SURFACE_STYLE_FILL_AREA ( #21161 ) ;
#5409 = CARTESIAN_POINT ( 'NONE',  ( -66.75560256528235925, 192.1022009597331817, 19.34154534151025118 ) ) ;
#5410 = AXIS2_PLACEMENT_3D ( 'NONE', #5812, #19823, #11126 ) ;
#5411 = EDGE_CURVE ( 'NONE', #4637, #20879, #1641, .T. ) ;
#5412 = ORIENTED_EDGE ( 'NONE', *, *, #17203, .T. ) ;
#5413 = EDGE_CURVE ( 'NONE', #19228, #10934, #7933, .T. ) ;
#5414 = ADVANCED_FACE ( 'NONE', ( #4252 ), #8777, .T. ) ;
#5415 = CARTESIAN_POINT ( 'NONE',  ( -10.85340889862633595, 73.95047783656255547, 127.4744267370078177 ) ) ;
#5416 = VERTEX_POINT ( 'NONE', #13462 ) ;
#5417 = ORIENTED_EDGE ( 'NONE', *, *, #15568, .F. ) ;
#5418 = ORIENTED_EDGE ( 'NONE', *, *, #6410, .T. ) ;
#5419 = ADVANCED_FACE ( 'NONE', ( #4357, #8276 ), #6336, .T. ) ;
#5420 = VECTOR ( 'NONE', #5787, 1000.000000000000000 ) ;
#5421 = APPLICATION_CONTEXT ( 'automotive_design' ) ;
#5422 = DIRECTION ( 'NONE',  ( -0.01292394549866739996, -0.005513023399721131770, -0.9999012842304692006 ) ) ;
#5424 = EDGE_LOOP ( 'NONE', ( #3370, #20935, #16893, #13245, #9677, #8824, #14554, #5406, #8907, #22526, #14174, #20482, #14940, #3307, #6283 ) ) ;
#5423 = ORIENTED_EDGE ( 'NONE', *, *, #5863, .F. ) ;
#5425 = EDGE_CURVE ( 'NONE', #7368, #4157, #17990, .T. ) ;
#5426 = CARTESIAN_POINT ( 'NONE',  ( -45.12496756436068068, 166.3499139106832558, 244.2261648130215690 ) ) ;
#5427 = CARTESIAN_POINT ( 'NONE',  ( -92.05960170301050027, 69.99999999999998579, 60.20821982323565180 ) ) ;
#5428 = TOROIDAL_SURFACE ( 'NONE', #19384, 4.400000000000000355, 0.4000000000000000222 ) ;
#5429 = CARTESIAN_POINT ( 'NONE',  ( -1.163172771417702478, 86.00000000000001421, -89.99248318111824574 ) ) ;
#5430 = CARTESIAN_POINT ( 'NONE',  ( -38.49583147354520918, 96.47889134396454835, 84.63024825845769783 ) ) ;
#5431 = ADVANCED_FACE ( 'NONE', ( #11383 ), #15076, .F. ) ;
#5432 = SURFACE_SIDE_STYLE ('',( #21178 ) ) ;
#5433 = CARTESIAN_POINT ( 'NONE',  ( 78.29383429238851022, 75.19279626719429643, -7.062306694037421728 ) ) ;
#5434 = CARTESIAN_POINT ( 'NONE',  ( 13.02529137814181048, 190.3775507350028136, 307.8631787466416085 ) ) ;
#5435 = CARTESIAN_POINT ( 'NONE',  ( 92.06552853299285744, 79.93537922958523723, 29.07356135706681499 ) ) ;
#5436 = AXIS2_PLACEMENT_3D ( 'NONE', #1552, #8538, #13841 ) ;
#5437 = EDGE_LOOP ( 'NONE', ( #11343, #3616, #3819, #21581 ) ) ;
#5438 = B_SPLINE_CURVE_WITH_KNOTS ( 'NONE', 3,
 ( #3384, #14317, #7057, #1677, #8651, #22635, #6932, #17526, #9001, #1779, #3603, #8756, #15810, #53, #14087, #5324, #12363, #19344, #8887, #10616, #17639, #7175, #398, #12585, #5433, #1894, #14205, #21179, #19454, #3719, #282, #19568, #3843, #21284, #17882, #2114, #21611, #9705, #16386, #5896, #21837, #14545, #12931 ),
 .UNSPECIFIED., .F., .F.,
 ( 4, 2, 2, 2, 2, 2, 2, 2, 1, 2, 2, 2, 2, 2, 2, 2, 2, 2, 2, 2, 2, 4 ),
 ( 0.000000000000000000, 0.001221601669963557615, 0.001832402504945335664, 0.002443203339927113929, 0.003664805009890686072, 0.004886406679854257348, 0.006108008349817829058, 0.006718809184799614045, 0.007329610019781399900, 0.007940410854763185755, 0.008551211689744970743, 0.009772813359708502554, 0.01099441502967203263, 0.01221601669963556618, 0.01282681753461733035, 0.01343761836959909625, 0.01465922003956262980, 0.01588082170952616334, 0.01649162254450792231, 0.01710242337948967781, 0.01832402504945320962, 0.01954562671941673449 ),
 .UNSPECIFIED. ) ;
#5439 = EDGE_CURVE ( 'NONE', #18197, #11858, #21917, .T. ) ;
#5440 = DIRECTION ( 'NONE',  ( 0.01292414190464131335, 1.902755938799530239E-22, 0.9999164797902015955 ) ) ;
#5441 = CARTESIAN_POINT ( 'NONE',  ( 17.46763696405603028, 137.6261247937603969, 113.4449059883549040 ) ) ;
#5442 = VERTEX_POINT ( 'NONE', #15198 ) ;
#5443 = CARTESIAN_POINT ( 'NONE',  ( -15.55823355279088638, 176.6145060706309380, 111.6566101476640114 ) ) ;
#5444 = CIRCLE ( 'NONE', #5457, 95.00000000000001421 ) ;
#5445 = ORIENTED_EDGE ( 'NONE', *, *, #16605, .T. ) ;
#5446 = AXIS2_PLACEMENT_3D ( 'NONE', #1468, #6625, #15496 ) ;
#5447 = LINE ( 'NONE', #20963, #9988 ) ;
#5448 = CARTESIAN_POINT ( 'NONE',  ( -44.75544497918918552, 164.1026264709444433, 19.21156598223192447 ) ) ;
#5449 = VERTEX_POINT ( 'NONE', #18512 ) ;
#5450 = DIRECTION ( 'NONE',  ( -0.01292414190464131335, -1.902755938799530239E-22, -0.9999164797902015955 ) ) ;
#5451 = LINE ( 'NONE', #21425, #19559 ) ;
#5452 = EDGE_CURVE ( 'NONE', #10697, #2793, #9781, .T. ) ;
#5453 = VERTEX_POINT ( 'NONE', #17357 ) ;
#5454 = CARTESIAN_POINT ( 'NONE',  ( 12.32651890270660644, 188.3103955803847782, 320.9483625192488034 ) ) ;
#5455 = ORIENTED_EDGE ( 'NONE', *, *, #16572, .T. ) ;
#5456 = DIRECTION ( 'NONE',  ( -0.01035335185279156155, -0.005513005182357613894, -0.9999312050732649393 ) ) ;
#5457 = AXIS2_PLACEMENT_3D ( 'NONE', #920, #8016, #8141 ) ;
#5458 = LINE ( 'NONE', #15842, #9540 ) ;
#5459 = VECTOR ( 'NONE', #6981, 1000.000000000000227 ) ;
#5460 = CARTESIAN_POINT ( 'NONE',  ( -55.90530736925617816, 114.7828611649933350, 163.2967483362970427 ) ) ;
#5461 = LINE ( 'NONE', #17681, #7007 ) ;
#5462 = ORIENTED_EDGE ( 'NONE', *, *, #11680, .F. ) ;
#5463 = CARTESIAN_POINT ( 'NONE',  ( -60.70062720570951598, 114.3921952957681185, 167.5133223899146344 ) ) ;
#5464 = ORIENTED_EDGE ( 'NONE', *, *, #19528, .T. ) ;
#5465 = EDGE_CURVE ( 'NONE', #14836, #11011, #7669, .T. ) ;
#5466 = CARTESIAN_POINT ( 'NONE',  ( -38.81891740251079170, 107.5014370005211504, 91.63662627299856922 ) ) ;
#5467 = CARTESIAN_POINT ( 'NONE',  ( 17.03779215356004073, 168.1915823533492755, 308.0767119223879718 ) ) ;
#5468 = SHAPE_REPRESENTATION ( 'Lower Angular Base Cradle Segment', ( #6292 ), #7758 ) ;
#5469 = CARTESIAN_POINT ( 'NONE',  ( -13.37948476813407872, 180.9346274286824325, 319.4053979151471481 ) ) ;
#5470 = CARTESIAN_POINT ( 'NONE',  ( 20.68288668254167462, 181.8935073550437664, 313.8768750210967369 ) ) ;
#5471 = ORIENTED_EDGE ( 'NONE', *, *, #20609, .F. ) ;
#5472 = AXIS2_PLACEMENT_3D ( 'NONE', #9423, #16243, #711 ) ;
#5473 =( GEOMETRIC_REPRESENTATION_CONTEXT ( 3 ) GLOBAL_UNCERTAINTY_ASSIGNED_CONTEXT ( ( #16447 ) ) GLOBAL_UNIT_ASSIGNED_CONTEXT ( ( #13592, #10248, #6903 ) ) REPRESENTATION_CONTEXT ( 'NONE', 'WORKASPACE' ) );
#5474 = CARTESIAN_POINT ( 'NONE',  ( -51.42803251223699590, 189.3893605493459233, -110.1610646708163159 ) ) ;
#5475 = ITEM_DEFINED_TRANSFORMATION ( 'NONE', 'NONE', #13591,  #6292 ) ;
#5476 = CARTESIAN_POINT ( 'NONE',  ( 39.45590449612061690, 92.86731729162988813, 83.62973377252751561 ) ) ;
#5477 = CIRCLE ( 'NONE', #3650, 2.000000000000002665 ) ;
#5478 = ORIENTED_EDGE ( 'NONE', *, *, #3039, .F. ) ;
#5479 = CARTESIAN_POINT ( 'NONE',  ( 1.175660927181459158E-14, 0.000000000000000000, 96.00000000000000000 ) ) ;
#5480 = ADVANCED_FACE ( 'NONE', ( #5148 ), #4129, .T. ) ;
#5481 = DIRECTION ( 'NONE',  ( 0.9999164797902015955, 2.001050586450178695E-22, -0.01292414190464131335 ) ) ;
#5482 = EDGE_CURVE ( 'NONE', #20680, #1571, #12906, .T. ) ;
#5483 = CARTESIAN_POINT ( 'NONE',  ( 49.39923347825703814, 108.3707227317548529, -46.80328957620831432 ) ) ;
#5484 = VERTEX_POINT ( 'NONE', #19836 ) ;
#5485 = DIRECTION ( 'NONE',  ( 0.01292394549866738955, 0.005513023399720468239, 0.9999012842304693116 ) ) ;
#5486 = CARTESIAN_POINT ( 'NONE',  ( -55.37125936483477773, 126.9053488551047053, 165.0682320037055320 ) ) ;
#5487 = ORIENTED_EDGE ( 'NONE', *, *, #1085, .T. ) ;
#5488 = LINE ( 'NONE', #14145, #7700 ) ;
#5489 = ORIENTED_EDGE ( 'NONE', *, *, #22256, .T. ) ;
#5490 = EDGE_LOOP ( 'NONE', ( #15549, #15181, #12571 ) ) ;
#5491 = CARTESIAN_POINT ( 'NONE',  ( 106.5693380255448091, 79.05027630924989523, 27.25937202119029124 ) ) ;
#5492 = CARTESIAN_POINT ( 'NONE',  ( -1.163172771417702700, 81.99999999999998579, -89.99248318111824574 ) ) ;
#5493 = CARTESIAN_POINT ( 'NONE',  ( 48.46580958134982353, 166.9169248112777666, 268.0158251802795917 ) ) ;
#5494 = CIRCLE ( 'NONE', #20525, 3.999999999999995559 ) ;
#5495 = VECTOR ( 'NONE', #18210, 1000.000000000000000 ) ;
#5496 = ORIENTED_EDGE ( 'NONE', *, *, #964, .F. ) ;
#5497 = ORIENTED_EDGE ( 'NONE', *, *, #20919, .F. ) ;
#5498 = DIRECTION ( 'NONE',  ( 0.003413786507418932210, -0.9644842718275384863, 0.2641182225045910492 ) ) ;
#5499 = PRODUCT_DEFINITION_FORMATION_WITH_SPECIFIED_SOURCE ( 'ANY', '', #9543, .NOT_KNOWN. ) ;
#5500 = PRODUCT_RELATED_PRODUCT_CATEGORY ( 'part', '', ( #15851 ) ) ;
#5501 = CARTESIAN_POINT ( 'NONE',  ( 0.2676632691968778843, 327.3448798950369110, 314.7619388544391654 ) ) ;
#5502 = CIRCLE ( 'NONE', #9558, 8.000000000000003553 ) ;
#5503 = CARTESIAN_POINT ( 'NONE',  ( 4.182528737366220106, 166.7840834110302808, 323.5943587238651276 ) ) ;
#5504 = VERTEX_POINT ( 'NONE', #12858 ) ;
#5505 = DIRECTION ( 'NONE',  ( 0.000000000000000000, 0.000000000000000000, -1.000000000000000000 ) ) ;
#5506 = CARTESIAN_POINT ( 'NONE',  ( -89.93579087582143927, 87.83132640396426893, 50.89035702524756033 ) ) ;
#5507 = VECTOR ( 'NONE', #4176, 1000.000000000000114 ) ;
#5508 = ORIENTED_EDGE ( 'NONE', *, *, #72, .F. ) ;
#5509 = AXIS2_PLACEMENT_3D ( 'NONE', #10719, #1995, #15677 ) ;
#5510 = EDGE_LOOP ( 'NONE', ( #11367, #9842, #10308, #515 ) ) ;
#5511 = LINE ( 'NONE', #9065, #11825 ) ;
#5512 = AXIS2_PLACEMENT_3D ( 'NONE', #18565, #11672, #13514 ) ;
#5513 = FACE_OUTER_BOUND ( 'NONE', #1951, .T. ) ;
#5514 = CARTESIAN_POINT ( 'NONE',  ( -49.00999508589215736, 110.7144623351035335, -43.54405342295051184 ) ) ;
#5515 = CARTESIAN_POINT ( 'NONE',  ( -106.1347175484142582, 70.98259407754899541, -28.90376667366510333 ) ) ;
#5516 = CARTESIAN_POINT ( 'NONE',  ( 93.21002351426729149, 77.12912189496647386, 28.79774562292276840 ) ) ;
#5517 = VERTEX_POINT ( 'NONE', #9043 ) ;
#5518 = DIRECTION ( 'NONE',  ( -0.9934404589540162256, -0.1135548637187056842, 0.01346653032743081423 ) ) ;
#5519 = CIRCLE ( 'NONE', #21296, 97.00000000000005684 ) ;
#5520 = ORIENTED_EDGE ( 'NONE', *, *, #6136, .T. ) ;
#5521 = DIRECTION ( 'NONE',  ( -0.000000000000000000, -1.000000000000000000, -0.000000000000000000 ) ) ;
#5522 = DIRECTION ( 'NONE',  ( -0.01292394549866738261, -0.005513023399719314648, -0.9999012842304692006 ) ) ;
#5523 = CARTESIAN_POINT ( 'NONE',  ( -76.19510332049942747, 75.05951099091890910, -2.385751844565587199 ) ) ;
#5524 = CARTESIAN_POINT ( 'NONE',  ( -12.75205171465932352, 164.7972115514004088, 311.1436431959231754 ) ) ;
#5525 = ORIENTED_EDGE ( 'NONE', *, *, #19905, .T. ) ;
#5526 = LINE ( 'NONE', #8862, #10670 ) ;
#5527 = CARTESIAN_POINT ( 'NONE',  ( -39.33507917608648086, 107.5562884034538769, 72.10905129613649933 ) ) ;
#5528 = CARTESIAN_POINT ( 'NONE',  ( -55.37247063347942344, 143.9050905090121546, 164.9745184335410499 ) ) ;
#5529 = B_SPLINE_CURVE_WITH_KNOTS ( 'NONE', 3,
 ( #5224, #8666, #21308, #5574, #10635, #21195 ),
 .UNSPECIFIED., .F., .F.,
 ( 4, 2, 4 ),
 ( 0.01452727543195646287, 0.01715716534226977355, 0.01978705525258308423 ),
 .UNSPECIFIED. ) ;
#5530 = DIRECTION ( 'NONE',  ( -0.01292394549866741384, -0.005513023399720269613, -0.9999012842304692006 ) ) ;
#5531 = VERTEX_POINT ( 'NONE', #10903 ) ;
#5532 = PRODUCT_DEFINITION_SHAPE ( 'NONE', 'NONE',  #22666 ) ;
#5533 = VECTOR ( 'NONE', #16393, 1000.000000000000000 ) ;
#5534 = EDGE_CURVE ( 'NONE', #5157, #21384, #16335, .T. ) ;
#5535 = ORIENTED_EDGE ( 'NONE', *, *, #20290, .T. ) ;
#5536 = DIRECTION ( 'NONE',  ( -7.125109674081160920E-05, 0.9999848031710253382, -0.005512562950849312846 ) ) ;
#5537 = ORIENTED_EDGE ( 'NONE', *, *, #15039, .T. ) ;
#5538 = CIRCLE ( 'NONE', #15118, 2.000000000000001332 ) ;
#5539 = EDGE_LOOP ( 'NONE', ( #17140, #15792 ) ) ;
#5540 = UNCERTAINTY_MEASURE_WITH_UNIT (LENGTH_MEASURE( 1.000000000000000082E-05 ), #14086, 'distance_accuracy_value', 'NONE');
#5541 = LINE ( 'NONE', #14194, #13756 ) ;
#5542 = VECTOR ( 'NONE', #9141, 1000.000000000000114 ) ;
#5543 = ORIENTED_EDGE ( 'NONE', *, *, #18624, .F. ) ;
#5544 = CYLINDRICAL_SURFACE ( 'NONE', #2531, 2.000000000000001332 ) ;
#5545 = CARTESIAN_POINT ( 'NONE',  ( -89.17419594629882340, 70.48718124881995095, 62.98708966501553874 ) ) ;
#5546 = CYLINDRICAL_SURFACE ( 'NONE', #21938, 6.000000000000000888 ) ;
#5547 = EDGE_CURVE ( 'NONE', #14225, #379, #5488, .T. ) ;
#5548 = DIRECTION ( 'NONE',  ( 0.9909299940865187173, -0.1338359446631173233, -0.01207007604876291287 ) ) ;
#5549 = CIRCLE ( 'NONE', #436, 8.000000000000005329 ) ;
#5550 = DIRECTION ( 'NONE',  ( 2.025474946048326158E-22, -1.000000000000000000, 1.876735158486679638E-22 ) ) ;
#5551 = EDGE_CURVE ( 'NONE', #9612, #10108, #7569, .T. ) ;
#5552 = ORIENTED_EDGE ( 'NONE', *, *, #2493, .F. ) ;
#5553 = CARTESIAN_POINT ( 'NONE',  ( 153.9999999999992610, 0.000000000000000000, -53.76161406891471017 ) ) ;
#5554 = FACE_OUTER_BOUND ( 'NONE', #18914, .T. ) ;
#5555 = AXIS2_PLACEMENT_3D ( 'NONE', #14855, #7587, #14620 ) ;
#5556 = CARTESIAN_POINT ( 'NONE',  ( 19.01596917749679250, 183.5201396444011266, 310.9998942482669690 ) ) ;
#5557 = FACE_OUTER_BOUND ( 'NONE', #3485, .T. ) ;
#5558 = ORIENTED_EDGE ( 'NONE', *, *, #17934, .T. ) ;
#5559 = VECTOR ( 'NONE', #20280, 1000.000000000000114 ) ;
#5560 = ADVANCED_FACE ( 'NONE', ( #5717 ), #8943, .F. ) ;
#5561 = CARTESIAN_POINT ( 'NONE',  ( -8.750674252510810547, 186.0658606611824553, 321.9654507654339000 ) ) ;
#5562 = CARTESIAN_POINT ( 'NONE',  ( -41.41899454747574083, 166.0889136240115249, 277.1829612759436827 ) ) ;
#5563 = ORIENTED_EDGE ( 'NONE', *, *, #16631, .T. ) ;
#5565 = CARTESIAN_POINT ( 'NONE',  ( -93.05058556066501296, 79.82257531472973255, -28.80218916741304014 ) ) ;
#5564 = AXIS2_PLACEMENT_3D ( 'NONE', #405, #3555, #19519 ) ;
#5566 = EDGE_LOOP ( 'NONE', ( #1546, #11711, #10545 ) ) ;
#5567 = AXIS2_PLACEMENT_3D ( 'NONE', #10893, #16658, #565 ) ;
#5568 = EDGE_CURVE ( 'NONE', #22376, #13705, #5494, .T. ) ;
#5569 = CARTESIAN_POINT ( 'NONE',  ( -1.749069042356333537, 70.09252763182293222, -99.14426119037081264 ) ) ;
#5570 = VECTOR ( 'NONE', #6901, 1000.000000000000000 ) ;
#5571 = SURFACE_STYLE_FILL_AREA ( #14332 ) ;
#5572 = PRODUCT_DEFINITION_CONTEXT ( 'detailed design', #17627, 'design' ) ;
#5573 = ORIENTED_EDGE ( 'NONE', *, *, #14869, .T. ) ;
#5574 = CARTESIAN_POINT ( 'NONE',  ( -8.125559787506135834, 70.35931727281543147, -83.29857057268348797 ) ) ;
#5575 = CARTESIAN_POINT ( 'NONE',  ( -10.78843133478213190, 106.5358177134646951, 133.7945456459338516 ) ) ;
#5576 = CARTESIAN_POINT ( 'NONE',  ( 93.17671387018316409, 79.04398536104964990, 26.22064129356684958 ) ) ;
#5577 = EDGE_CURVE ( 'NONE', #5930, #19051, #14321, .T. ) ;
#5578 = VERTEX_POINT ( 'NONE', #14495 ) ;
#5579 = CARTESIAN_POINT ( 'NONE',  ( 12.18842727924546665, 188.3644011796234565, 320.9609158465759720 ) ) ;
#5580 = VERTEX_POINT ( 'NONE', #5373 ) ;
#5581 = AXIS2_PLACEMENT_3D ( 'NONE', #15250, #13737, #11781 ) ;
#5582 = DIRECTION ( 'NONE',  ( -7.125109674161231961E-05, 0.9999848031710252272, -0.005512562950850142043 ) ) ;
#5583 = CIRCLE ( 'NONE', #19524, 6.000000000000000888 ) ;
#5584 = CARTESIAN_POINT ( 'NONE',  ( 66.73173682738227797, 70.03297899285537653, -87.44705638319801722 ) ) ;
#5585 = SURFACE_STYLE_FILL_AREA ( #21094 ) ;
#5586 = CARTESIAN_POINT ( 'NONE',  ( -40.92874639037903961, 94.48610424851698042, 83.92603509844954601 ) ) ;
#5587 = DIRECTION ( 'NONE',  ( 7.125109674160258889E-05, -0.9999848031710252272, 0.005512562950849897447 ) ) ;
#5588 = EDGE_LOOP ( 'NONE', ( #5762, #16200 ) ) ;
#5589 = CARTESIAN_POINT ( 'NONE',  ( -59.95575053096360563, 114.2084250825692209, 165.7205294013835157 ) ) ;
#5590 = ORIENTED_EDGE ( 'NONE', *, *, #10621, .F. ) ;
#5591 = CARTESIAN_POINT ( 'NONE',  ( -66.06691928577359363, 94.02752048664900997, -82.12548041065298321 ) ) ;
#5592 = AXIS2_PLACEMENT_3D ( 'NONE', #19279, #14139, #333 ) ;
#5593 = CARTESIAN_POINT ( 'NONE',  ( -2.342497703613107607, 327.0213694383911047, 308.5633357006506117 ) ) ;
#5594 = CARTESIAN_POINT ( 'NONE',  ( -15.43087866951515608, 177.9355826206890470, 316.4028962195858981 ) ) ;
#5595 = CLOSED_SHELL ( 'NONE', ( #12878, #13645, #14943, #6102, #6007, #15044, #17153, #12032, #21907, #21432, #6595, #3880, #15291, #8663, #13433, #2528, #19793, #7266, #15208, #17634, #12850, #8224, #13384, #15735, #4898, #13072, #12730, #4707, #14555, #18809, #21290, #2011, #2089, #7209, #6181, #2034, #6609, #13874, #4371, #8551, #16216, #16968, #9118, #16804, #4635, #11894, #1299, #18687, #14657, #5011, #17094, #15704, #1980, #3181, #20501, #4045, #5967, #5688, #16959, #11030, #11115, #3738, #5291, #20121, #19644, #9389, #13567, #17516, #16935, #4669, #21786, #7810, #11886, #1936, #5414, #16672, #2621, #21549, #3798, #22252, #4572, #12743, #12880, #7281, #9219, #12193, #12635, #19916 ) ) ;
#5596 = DIRECTION ( 'NONE',  ( -0.9999164797902017066, -2.001050586450178931E-22, 0.01292414190464131508 ) ) ;
#5597 = ADVANCED_FACE ( 'NONE', ( #12412 ), #15052, .F. ) ;
#5598 = ORIENTED_EDGE ( 'NONE', *, *, #22301, .T. ) ;
#5599 = VECTOR ( 'NONE', #20292, 1000.000000000000114 ) ;
#5600 = VECTOR ( 'NONE', #4754, 1000.000000000000114 ) ;
#5601 = DIRECTION ( 'NONE',  ( -0.01292394549866741557, -0.005513023399720270480, -0.9999012842304693116 ) ) ;
#5602 = CARTESIAN_POINT ( 'NONE',  ( 41.09521125350259041, 69.99999999999998579, 84.47593510598149180 ) ) ;
#5603 = EDGE_CURVE ( 'NONE', #959, #44, #4376, .T. ) ;
#5604 = DIRECTION ( 'NONE',  ( 0.8981428216242065554, 0.000000000000000000, -0.4397038457472354223 ) ) ;
#5605 = CARTESIAN_POINT ( 'NONE',  ( 49.95329303650502339, 110.8261100212978363, -47.70120114633578368 ) ) ;
#5606 = ORIENTED_EDGE ( 'NONE', *, *, #22283, .T. ) ;
#5607 = VECTOR ( 'NONE', #20536, 1000.000000000000000 ) ;
#5608 = VERTEX_POINT ( 'NONE', #16098 ) ;
#5609 = CARTESIAN_POINT ( 'NONE',  ( 89.47454773680249218, 97.89961987228680584, -63.98691110171232310 ) ) ;
#5610 = CARTESIAN_POINT ( 'NONE',  ( -52.23863840496477451, 118.9192529882356126, 167.5720208779842153 ) ) ;
#5611 = CARTESIAN_POINT ( 'NONE',  ( 79.99331838321626265, 102.0000000000000000, -7.033931352371318724 ) ) ;
#5612 = VERTEX_POINT ( 'NONE', #14375 ) ;
#5613 = ORIENTED_EDGE ( 'NONE', *, *, #4206, .T. ) ;
#5614 = DIRECTION ( 'NONE',  ( 7.125109674160258889E-05, -0.9999848031710252272, 0.005512562950849896580 ) ) ;
#5615 = CARTESIAN_POINT ( 'NONE',  ( 12.81118841006561304, 189.7386529835138731, 320.9279672944379058 ) ) ;
#5616 = CARTESIAN_POINT ( 'NONE',  ( -44.25520882077128704, 168.2183454221810734, 273.2074843050344271 ) ) ;
#5617 = PLANE ( 'NONE',  #16249 ) ;
#5618 = CONICAL_SURFACE ( 'NONE', #4885, 5.700000000000001954, 0.7853981633974482790 ) ;
#5619 = AXIS2_PLACEMENT_3D ( 'NONE', #15998, #19404, #17364 ) ;
#5620 = ORIENTED_EDGE ( 'NONE', *, *, #1256, .F. ) ;
#5621 = CARTESIAN_POINT ( 'NONE',  ( -64.64710546055418661, 118.1474297122748709, 27.72283698990772649 ) ) ;
#5622 = CARTESIAN_POINT ( 'NONE',  ( 2.830031787867828275, 81.19615242270661781, -80.39798906481894392 ) ) ;
#5623 = EDGE_CURVE ( 'NONE', #21384, #11064, #21341, .T. ) ;
#5624 = ADVANCED_FACE ( 'NONE', ( #19619 ), #2186, .F. ) ;
#5625 = VERTEX_POINT ( 'NONE', #21455 ) ;
#5626 = CIRCLE ( 'NONE', #1603, 1.999999999999997780 ) ;
#5627 = CARTESIAN_POINT ( 'NONE',  ( 0.000000000000000000, 20.00000000000000000, 0.000000000000000000 ) ) ;
#5628 = CARTESIAN_POINT ( 'NONE',  ( -88.17009401808903135, 88.77120466299882651, 52.29915554423978818 ) ) ;
#5629 = DIRECTION ( 'NONE',  ( -0.3503253878659050580, 0.9365298858406040372, -0.01356080911997331606 ) ) ;
#5630 = VECTOR ( 'NONE', #12093, 999.9999999999998863 ) ;
#5631 = ORIENTED_EDGE ( 'NONE', *, *, #14699, .T. ) ;
#5632 = CIRCLE ( 'NONE', #10403, 3.399999999999986144 ) ;
#5633 = ORIENTED_EDGE ( 'NONE', *, *, #8536, .F. ) ;
#5634 = LINE ( 'NONE', #477, #12180 ) ;
#5635 = CARTESIAN_POINT ( 'NONE',  ( -14.82979117956944037, 177.4987173824078468, 90.64024647396865930 ) ) ;
#5636 = CARTESIAN_POINT ( 'NONE',  ( -46.77031037318527495, 119.7725967263615985, 250.1981111634296155 ) ) ;
#5637 = DIRECTION ( 'NONE',  ( 0.01292414190464131335, 0.000000000000000000, 0.9999164797902017066 ) ) ;
#5638 = ORIENTED_EDGE ( 'NONE', *, *, #15278, .F. ) ;
#5639 = CARTESIAN_POINT ( 'NONE',  ( 3.316624388958365088, 166.4147108432491109, 256.6009726804241495 ) ) ;
#5640 = VERTEX_POINT ( 'NONE', #11590 ) ;
#5641 = LINE ( 'NONE', #19751, #12888 ) ;
#5642 = FACE_OUTER_BOUND ( 'NONE', #2960, .T. ) ;
#5643 = AXIS2_PLACEMENT_3D ( 'NONE', #11511, #15529, #8946 ) ;
#5644 = CARTESIAN_POINT ( 'NONE',  ( 51.64670511766545502, 78.91761970611437960, -27.66980033337678790 ) ) ;
#5645 = CARTESIAN_POINT ( 'NONE',  ( -7.728110352850903197, 165.4125665588315144, 321.2590829791397482 ) ) ;
#5646 = CARTESIAN_POINT ( 'NONE',  ( 3.872354045398203937, 166.6517708494369856, 299.5967279023338392 ) ) ;
#5647 = EDGE_LOOP ( 'NONE', ( #19643, #19545, #12569, #8314 ) ) ;
#5648 = CARTESIAN_POINT ( 'NONE',  ( -36.15575339682945355, 93.60246143706251587, -82.12095408908095351 ) ) ;
#5649 = CARTESIAN_POINT ( 'NONE',  ( -7.798485590386966315, 81.43869406011346257, -82.51270763647201534 ) ) ;
#5650 = VECTOR ( 'NONE', #4645, 1000.000000000000000 ) ;
#5651 = CARTESIAN_POINT ( 'NONE',  ( -51.17267260618272218, 110.8317321599929244, -46.39618586169468983 ) ) ;
#5652 = VERTEX_POINT ( 'NONE', #20067 ) ;
#5653 = FACE_OUTER_BOUND ( 'NONE', #4377, .T. ) ;
#5654 = VERTEX_POINT ( 'NONE', #16664 ) ;
#5655 = VERTEX_POINT ( 'NONE', #916 ) ;
#5656 = LINE ( 'NONE', #19217, #14875 ) ;
#5657 = AXIS2_PLACEMENT_3D ( 'NONE', #10429, #1928, #7085 ) ;
#5658 = VERTEX_POINT ( 'NONE', #11693 ) ;
#5659 = DIRECTION ( 'NONE',  ( -2.025474946048326158E-22, 1.000000000000000000, -1.876735158486679638E-22 ) ) ;
#5660 = CARTESIAN_POINT ( 'NONE',  ( 19.43891449096291169, 175.6145212674599065, 111.2097777439524151 ) ) ;
#5661 = AXIS2_PLACEMENT_3D ( 'NONE', #17166, #13838, #18771 ) ;
#5662 = CARTESIAN_POINT ( 'NONE',  ( 6.473302864968231596, 70.07547478993376444, -95.06675942850822025 ) ) ;
#5663 = DIRECTION ( 'NONE',  ( -0.4397038457472432493, 0.000000000000000000, -0.8981428216242028917 ) ) ;
#5664 = LINE ( 'NONE', #9704, #14701 ) ;
#5665 = DIRECTION ( 'NONE',  ( 1.000000000000000000, -0.000000000000000000, -1.458023040593674599E-16 ) ) ;
#5666 = CARTESIAN_POINT ( 'NONE',  ( 11.87914702380516019, 187.7661313520924296, 307.7599159327405687 ) ) ;
#5667 = CARTESIAN_POINT ( 'NONE',  ( 52.34460878051607580, 84.99999999999997158, 26.32568957529409204 ) ) ;
#5668 = DIRECTION ( 'NONE',  ( 0.9999164797902017066, 2.001050586450178931E-22, -0.01292414190464131508 ) ) ;
#5669 = EDGE_LOOP ( 'NONE', ( #1341, #2252, #7969, #14032, #7123, #19464 ) ) ;
#5670 = AXIS2_PLACEMENT_3D ( 'NONE', #20814, #1655, #5304 ) ;
#5671 = CARTESIAN_POINT ( 'NONE',  ( 39.42082737383938706, 91.17157287525387233, -83.51645567887783272 ) ) ;
#5672 = DIRECTION ( 'NONE',  ( 0.9999164797902015955, 8.772500386246550856E-18, -0.01292414190464154927 ) ) ;
#5673 = EDGE_LOOP ( 'NONE', ( #19325, #12436, #20264 ) ) ;
#5674 = DIRECTION ( 'NONE',  ( -0.01292394549866738608, -0.005513023399720699824, -0.9999012842304692006 ) ) ;
#5675 = EDGE_CURVE ( 'NONE', #1967, #17055, #21882, .T. ) ;
#5676 = VERTEX_POINT ( 'NONE', #2954 ) ;
#5677 = EDGE_CURVE ( 'NONE', #14965, #7858, #15797, .T. ) ;
#5678 = ORIENTED_EDGE ( 'NONE', *, *, #8353, .T. ) ;
#5679 = DIRECTION ( 'NONE',  ( -0.9909299940865188283, 0.1338359446631172955, 0.01207007604876741101 ) ) ;
#5680 = DIRECTION ( 'NONE',  ( -0.1288482667915161195, -1.253717443260671070E-17, 0.9916643202943334900 ) ) ;
#5681 = AXIS2_PLACEMENT_3D ( 'NONE', #13803, #8490, #17481 ) ;
#5682 = ORIENTED_EDGE ( 'NONE', *, *, #9855, .T. ) ;
#5683 = DIRECTION ( 'NONE',  ( -0.9999164797902017066, -2.001050586450177990E-22, 0.01292414190464177999 ) ) ;
#5684 = CARTESIAN_POINT ( 'NONE',  ( 0.000000000000000000, 18.00000000000000355, 0.000000000000000000 ) ) ;
#5685 = EDGE_CURVE ( 'NONE', #13983, #21156, #1016, .T. ) ;
#5686 = FACE_OUTER_BOUND ( 'NONE', #9770, .T. ) ;
#5687 = ORIENTED_EDGE ( 'NONE', *, *, #21314, .F. ) ;
#5688 = ADVANCED_FACE ( 'NONE', ( #2846 ), #16877, .T. ) ;
#5689 = CARTESIAN_POINT ( 'NONE',  ( 12.27027136777087790, 187.6773065828753602, 322.9709648702423692 ) ) ;
#5690 = VERTEX_POINT ( 'NONE', #6420 ) ;
#5691 = EDGE_LOOP ( 'NONE', ( #10486, #5346, #20115, #1205 ) ) ;
#5692 = DIRECTION ( 'NONE',  ( 1.000000000000000000, 0.000000000000000000, 0.000000000000000000 ) ) ;
#5693 = LINE ( 'NONE', #19364, #7860 ) ;
#5694 = ADVANCED_FACE ( 'NONE', ( #683 ), #7672, .T. ) ;
#5695 = DIRECTION ( 'NONE',  ( 0.01292414190464131508, 0.000000000000000000, 0.9999164797902017066 ) ) ;
#5696 = CARTESIAN_POINT ( 'NONE',  ( -8.650559030193861076, 185.1599980327158335, 323.2452797403996101 ) ) ;
#5697 = CARTESIAN_POINT ( 'NONE',  ( -91.90296438722893413, 77.16966923688050883, 31.25747399733658938 ) ) ;
#5698 = DIRECTION ( 'NONE',  ( 7.125109674160258889E-05, -0.9999848031710252272, 0.005512562950849896580 ) ) ;
#5699 = ORIENTED_EDGE ( 'NONE', *, *, #8354, .T. ) ;
#5700 = CARTESIAN_POINT ( 'NONE',  ( -14.48915200586460372, 181.2968306206680325, 311.4287039645396931 ) ) ;
#5701 = CARTESIAN_POINT ( 'NONE',  ( -164.0000000000000000, 18.00000000000000355, 8.000000000000019540 ) ) ;
#5702 = CARTESIAN_POINT ( 'NONE',  ( -15.10148691740612747, 178.5546173124768927, 314.7004641218159691 ) ) ;
#5703 = ORIENTED_EDGE ( 'NONE', *, *, #349, .T. ) ;
#5704 = CIRCLE ( 'NONE', #19998, 102.6746853779045381 ) ;
#5705 = EDGE_CURVE ( 'NONE', #2340, #12564, #20896, .T. ) ;
#5706 = CARTESIAN_POINT ( 'NONE',  ( -46.78944003694669362, 119.3672327899910073, 248.7180851633275438 ) ) ;
#5707 = EDGE_CURVE ( 'NONE', #12309, #10802, #13942, .T. ) ;
#5708 = ORIENTED_EDGE ( 'NONE', *, *, #20157, .T. ) ;
#5709 = EDGE_CURVE ( 'NONE', #6772, #18256, #22229, .T. ) ;
#5710 = CARTESIAN_POINT ( 'NONE',  ( 45.23725195521918607, 161.1026720614313206, 18.06493089966673082 ) ) ;
#5711 = DIRECTION ( 'NONE',  ( -7.125109674403837105E-05, 0.9999848031710252272, -0.005512562950847867821 ) ) ;
#5712 = CARTESIAN_POINT ( 'NONE',  ( 49.87189298987733110, 110.6628876857999302, -47.64038739181492588 ) ) ;
#5713 = VERTEX_POINT ( 'NONE', #8253 ) ;
#5714 = CARTESIAN_POINT ( 'NONE',  ( -41.94137166082473556, 162.5796238295972671, 273.2086669205137355 ) ) ;
#5715 = VERTEX_POINT ( 'NONE', #19136 ) ;
#5716 = ADVANCED_FACE ( 'NONE', ( #6521 ), #12033, .T. ) ;
#5717 = FACE_OUTER_BOUND ( 'NONE', #18952, .T. ) ;
#5718 = VERTEX_POINT ( 'NONE', #1700 ) ;
#5719 = PLANE ( 'NONE',  #1202 ) ;
#5720 = CARTESIAN_POINT ( 'NONE',  ( -164.0000000000000284, 0.8284271247461896248, -7.999999999999978684 ) ) ;
#5721 = DIRECTION ( 'NONE',  ( 0.000000000000000000, 0.000000000000000000, 1.000000000000000000 ) ) ;
#5722 = CARTESIAN_POINT ( 'NONE',  ( -28.61234839824397369, 91.18282421267417703, 80.66236699840530378 ) ) ;
#5723 = ORIENTED_EDGE ( 'NONE', *, *, #13617, .T. ) ;
#5724 = DIRECTION ( 'NONE',  ( 0.01292394549866743465, 0.005513023399721021615, 0.9999012842304692006 ) ) ;
#5725 = CARTESIAN_POINT ( 'NONE',  ( -2.180642712250696835, 81.85301533877169788, -99.20033613248658355 ) ) ;
#5726 = EDGE_CURVE ( 'NONE', #19075, #9610, #22335, .T. ) ;
#5727 = ORIENTED_EDGE ( 'NONE', *, *, #22223, .T. ) ;
#5728 = CARTESIAN_POINT ( 'NONE',  ( 41.32970315430851826, 107.3915281860326871, 70.92239337605512617 ) ) ;
#5729 = DIRECTION ( 'NONE',  ( 0.000000000000000000, 1.000000000000000000, -0.000000000000000000 ) ) ;
#5730 = PRODUCT_CONTEXT ( 'NONE', #4551, 'mechanical' ) ;
#5732 = ORIENTED_EDGE ( 'NONE', *, *, #11214, .F. ) ;
#5731 = ORIENTED_EDGE ( 'NONE', *, *, #62, .T. ) ;
#5733 = CARTESIAN_POINT ( 'NONE',  ( -90.17421880070757823, 70.18950621168607995, 62.99705530356752803 ) ) ;
#5734 = EDGE_LOOP ( 'NONE', ( #1233, #16746, #12694, #19620 ) ) ;
#5735 = LINE ( 'NONE', #15, #22424 ) ;
#5736 =( BOUNDED_SURFACE ( )  B_SPLINE_SURFACE ( 3, 2, ( 
 ( #21176, #12241, #15690 ),
 ( #22633, #17637, #17524 ),
 ( #21068, #8753, #5322 ),
 ( #3602, #21281, #19451 ),
 ( #16156, #12581, #12359 ),
 ( #1890, #15930, #2010 ),
 ( #17767, #178, #16044 ),
 ( #5430, #280, #17879 ),
 ( #7275, #14313, #2112 ),
 ( #9104, #395, #16273 ),
 ( #9700, #16722, #5767 ),
 ( #969, #21502, #863 ),
 ( #11537, #21609, #2570 ),
 ( #2345, #741, #9578 ),
 ( #6014, #18100, #7738 ),
 ( #7955, #20243, #14989 ) ),
 .UNSPECIFIED., .F., .F., .T. ) 
 B_SPLINE_SURFACE_WITH_KNOTS ( ( 4, 2, 2, 2, 2, 2, 2, 4 ),
 ( 3, 3 ),
 ( 0.01296814958356296704, 0.01375736145185813344, 0.01454657332015329985, 0.01533578518844846625, 0.01612499705674363265, 0.01691420892503879905, 0.01770342079333396546, 0.01928184452992429826 ),
 ( 0.000000000000000000, 1.000000000000000000 ),
 .UNSPECIFIED. ) 
 GEOMETRIC_REPRESENTATION_ITEM ( )  RATIONAL_B_SPLINE_SURFACE ( (
 ( 1.000000000000000000, 0.7071067811865456854, 1.000000000000000000),
 ( 1.000000000000000000, 0.7085856290790960577, 1.000000000000000000),
 ( 1.000000000000000000, 0.7100245998945194925, 1.000000000000000000),
 ( 1.000000000000000000, 0.7128280673175965143, 1.000000000000000000),
 ( 1.000000000000000000, 0.7142069464324342087, 1.000000000000000000),
 ( 1.000000000000000000, 0.7168109644888088772, 1.000000000000000000),
 ( 1.000000000000000000, 0.7180337263083194088, 1.000000000000000000),
 ( 1.000000000000000000, 0.7203292399658924872, 1.000000000000000000),
 ( 1.000000000000000000, 0.7214053064842161911, 1.000000000000000000),
 ( 1.000000000000000000, 0.7233195371734718604, 1.000000000000000000),
 ( 1.000000000000000000, 0.7241710127918253859, 1.000000000000000000),
 ( 1.000000000000000000, 0.7256648496837366791, 1.000000000000000000),
 ( 1.000000000000000000, 0.7262924578673953802, 1.000000000000000000),
 ( 1.000000000000000000, 0.7277939499224679309, 1.000000000000000000),
 ( 1.000000000000000000, 0.7283089038925458780, 1.000000000000000000),
 ( 1.000000000000000000, 0.7282773916567022443, 1.000000000000000000) ) ) 
 REPRESENTATION_ITEM ( '' )  SURFACE ( )  );
#5737 = CARTESIAN_POINT ( 'NONE',  ( 79.99331838321626265, 55.99999999999999289, -1.033931352371318058 ) ) ;
#5738 = ORIENTED_EDGE ( 'NONE', *, *, #1966, .F. ) ;
#5739 = LINE ( 'NONE', #5857, #11238 ) ;
#5740 = DIRECTION ( 'NONE',  ( 7.125109674161246868E-05, -0.9999848031710252272, 0.005512562950850154186 ) ) ;
#5741 = DIRECTION ( 'NONE',  ( 0.9999164797902017066, 2.001050586450178931E-22, -0.01292414190464131508 ) ) ;
#5742 = VERTEX_POINT ( 'NONE', #20642 ) ;
#5743 = ADVANCED_FACE ( 'NONE', ( #15280 ), #13538, .F. ) ;
#5744 = CYLINDRICAL_SURFACE ( 'NONE', #12830, 110.0000000000000000 ) ;
#5745 = ORIENTED_EDGE ( 'NONE', *, *, #22642, .F. ) ;
#5746 = CARTESIAN_POINT ( 'NONE',  ( -163.1715728752537871, 20.00000000000000000, 8.828427124746209387 ) ) ;
#5747 = DIRECTION ( 'NONE',  ( 0.9999164797902017066, 0.000000000000000000, -0.01292414190464177826 ) ) ;
#5748 = CARTESIAN_POINT ( 'NONE',  ( 106.2770331005257702, 78.91761970611437960, -28.37590941890325880 ) ) ;
#5749 = CYLINDRICAL_SURFACE ( 'NONE', #4073, 7.499999999999991118 ) ;
#5750 = CARTESIAN_POINT ( 'NONE',  ( -55.33837949231439524, 118.9192529882355984, 167.6120857178885899 ) ) ;
#5751 = DIRECTION ( 'NONE',  ( 7.125109674403277385E-05, -0.9999848031710253382, 0.005512562950848281552 ) ) ;
#5752 = DIRECTION ( 'NONE',  ( 0.5121193912974630891, -0.6668151060996335699, 0.5413791123920929094 ) ) ;
#5753 = B_SPLINE_CURVE_WITH_KNOTS ( 'NONE', 3,
 ( #9194, #13122, #11618, #20092, #16582, #18284, #10004 ),
 .UNSPECIFIED., .F., .F.,
 ( 4, 3, 4 ),
 ( 0.000000000000000000, 0.004771063351880659026, 0.01050764680140206173 ),
 .UNSPECIFIED. ) ;
#5754 = DIRECTION ( 'NONE',  ( 7.125109674364534776E-05, -0.9999848031710252272, 0.005512562950849704893 ) ) ;
#5755 = VERTEX_POINT ( 'NONE', #6631 ) ;
#5756 = CARTESIAN_POINT ( 'NONE',  ( -146.5000000000000000, 0.000000000000000000, 10.00000000000001599 ) ) ;
#5757 = FACE_OUTER_BOUND ( 'NONE', #1245, .T. ) ;
#5758 = ORIENTED_EDGE ( 'NONE', *, *, #11338, .T. ) ;
#5759 = VERTEX_POINT ( 'NONE', #9974 ) ;
#5760 = CARTESIAN_POINT ( 'NONE',  ( -83.16258572756845524, 75.08619966718656258, -2.975792177979545983 ) ) ;
#5761 = CARTESIAN_POINT ( 'NONE',  ( -90.13276696777731445, 88.30345154740933822, 52.91026065720622285 ) ) ;
#5762 = ORIENTED_EDGE ( 'NONE', *, *, #8689, .F. ) ;
#5763 = CIRCLE ( 'NONE', #9429, 7.499999999999992006 ) ;
#5764 = DIRECTION ( 'NONE',  ( -0.08947859377482220156, 0.6986239096456045017, -0.7098719702365846596 ) ) ;
#5765 = LINE ( 'NONE', #5660, #17593 ) ;
#5766 = CARTESIAN_POINT ( 'NONE',  ( 6.808509919968707358, 69.99999999999998579, -94.26135563083261104 ) ) ;
#5767 = CARTESIAN_POINT ( 'NONE',  ( -39.34031886361867691, 93.71576119831708240, 84.68445348450920562 ) ) ;
#5768 = ADVANCED_FACE ( 'NONE', ( #4899 ), #10427, .F. ) ;
#5769 = DIRECTION ( 'NONE',  ( -0.000000000000000000, -1.000000000000000000, -0.000000000000000000 ) ) ;
#5770 = CARTESIAN_POINT ( 'NONE',  ( 11.33842039275930347, 189.5802358106135159, 275.5617015998586794 ) ) ;
#5771 = CARTESIAN_POINT ( 'NONE',  ( 17.89548223907189950, 186.1632423467296462, 310.0097253882542532 ) ) ;
#5772 = CARTESIAN_POINT ( 'NONE',  ( 84.36252974213543609, 104.9530375760216714, 70.59083440939240006 ) ) ;
#5773 = DIRECTION ( 'NONE',  ( 0.8981428216242086648, -0.000000000000000000, 0.4397038457472312589 ) ) ;
#5774 = ORIENTED_EDGE ( 'NONE', *, *, #1053, .F. ) ;
#5775 =( LENGTH_UNIT ( ) NAMED_UNIT ( * ) SI_UNIT ( .MILLI., .METRE. ) );
#5776 = VECTOR ( 'NONE', #10122, 1000.000000000000114 ) ;
#5777 = LINE ( 'NONE', #12475, #4046 ) ;
#5778 = CARTESIAN_POINT ( 'NONE',  ( -10.02115732914335489, 187.8727529749444045, 308.1601390762862138 ) ) ;
#5779 = ORIENTED_EDGE ( 'NONE', *, *, #5841, .F. ) ;
#5780 = DIRECTION ( 'NONE',  ( 0.4397038457472354778, 0.000000000000000000, -0.8981428216242066664 ) ) ;
#5781 = ORIENTED_EDGE ( 'NONE', *, *, #2199, .F. ) ;
#5782 = PRODUCT_DEFINITION ( 'UNKNOWN', '', #20169, #12262 ) ;
#5783 = DIRECTION ( 'NONE',  ( -0.8504393858994485633, 0.002839416958724588855, 0.5260653843604455870 ) ) ;
#5784 = AXIS2_PLACEMENT_3D ( 'NONE', #16710, #4033, #2557 ) ;
#5785 = CARTESIAN_POINT ( 'NONE',  ( -36.55288090549052527, 94.02752048664899576, 83.45186405039063970 ) ) ;
#5786 = CARTESIAN_POINT ( 'NONE',  ( 24.36720253925702906, 95.51270090492251086, 81.35618551405543997 ) ) ;
#5787 = DIRECTION ( 'NONE',  ( 7.176269450075762180E-19, -1.000000000000000000, 5.550596000020001457E-17 ) ) ;
#5788 = CARTESIAN_POINT ( 'NONE',  ( -90.51228951533471445, 70.60983096564289951, 62.93517888374829994 ) ) ;
#5789 = PRODUCT_DEFINITION_CONTEXT ( 'detailed design', #7783, 'design' ) ;
#5790 = CARTESIAN_POINT ( 'NONE',  ( -38.56600193350200811, 165.4640537929580830, 244.1462729796548103 ) ) ;
#5791 = CARTESIAN_POINT ( 'NONE',  ( 163.9999999999998863, 1.999999999999998224, -8.000000000002268408 ) ) ;
#5792 = AXIS2_PLACEMENT_3D ( 'NONE', #14456, #14218, #19470 ) ;
#5793 = CARTESIAN_POINT ( 'NONE',  ( -7.475646132950445555, 81.99999999999998579, -81.73701953211951832 ) ) ;
#5794 = ORIENTED_EDGE ( 'NONE', *, *, #7471, .F. ) ;
#5795 = ORIENTED_EDGE ( 'NONE', *, *, #13085, .T. ) ;
#5796 = DIRECTION ( 'NONE',  ( 0.9008530678525494828, -0.002400200757025988674, -0.4341174831505594800 ) ) ;
#5797 = DIRECTION ( 'NONE',  ( -0.01292394549866740343, -0.005513023399721215904, -0.9999012842304693116 ) ) ;
#5798 = ADVANCED_FACE ( 'NONE', ( #17201 ), #22342, .T. ) ;
#5799 = CARTESIAN_POINT ( 'NONE',  ( -44.65237404513518271, 168.6466622724118452, 27.18596972279685531 ) ) ;
#5800 = CARTESIAN_POINT ( 'NONE',  ( -14.37443239621853408, 105.6999454642524654, 127.3358366182947634 ) ) ;
#5802 = LINE ( 'NONE', #12836, #8382 ) ;
#5801 = CARTESIAN_POINT ( 'NONE',  ( -90.65403358069494288, 80.14440291447093045, 32.01641220276452771 ) ) ;
#5803 = FACE_BOUND ( 'NONE', #5588, .T. ) ;
#5804 = ORIENTED_EDGE ( 'NONE', *, *, #21259, .F. ) ;
#5805 = CIRCLE ( 'NONE', #18656, 2.000000000000001332 ) ;
#5806 = DIRECTION ( 'NONE',  ( -0.8981428216242027807, -0.000000000000000000, 0.4397038457472431938 ) ) ;
#5807 = CARTESIAN_POINT ( 'NONE',  ( -101.0000000000000000, 37.00000000000000711, 0.000000000000000000 ) ) ;
#5808 = CARTESIAN_POINT ( 'NONE',  ( -15.36585396882763277, 178.1140882805800345, 312.4503017070314286 ) ) ;
#5809 = AXIS2_PLACEMENT_3D ( 'NONE', #17411, #1769, #3597 ) ;
#5810 = ORIENTED_EDGE ( 'NONE', *, *, #4636, .F. ) ;
#5811 = VERTEX_POINT ( 'NONE', #20859 ) ;
#5812 = CARTESIAN_POINT ( 'NONE',  ( -55.34016076973275489, 143.9188730675114414, 167.4742716441172377 ) ) ;
#5813 = EDGE_CURVE ( 'NONE', #15229, #1291, #18902, .T. ) ;
#5814 = ORIENTED_EDGE ( 'NONE', *, *, #8533, .F. ) ;
#5815 = CARTESIAN_POINT ( 'NONE',  ( 39.39497909003009823, 72.00000000000000000, -85.51628863845822082 ) ) ;
#5816 = EDGE_CURVE ( 'NONE', #18739, #20005, #16886, .T. ) ;
#5817 = ITEM_DEFINED_TRANSFORMATION ( 'NONE', 'NONE', #6606,  #6292 ) ;
#5818 = VECTOR ( 'NONE', #18808, 999.9999999999998863 ) ;
#5819 = DIRECTION ( 'NONE',  ( -0.01292394549866738261, -0.005513023399719314648, -0.9999012842304692006 ) ) ;
#5820 = VECTOR ( 'NONE', #7344, 1000.000000000000114 ) ;
#5821 = CARTESIAN_POINT ( 'NONE',  ( -44.49988481842636645, 152.0384941537814427, 275.3698588368105789 ) ) ;
#5822 = EDGE_CURVE ( 'NONE', #4506, #17671, #19782, .T. ) ;
#5823 = ORIENTED_EDGE ( 'NONE', *, *, #11174, .F. ) ;
#5824 = EDGE_CURVE ( 'NONE', #22379, #18446, #7387, .T. ) ;
#5825 = FACE_BOUND ( 'NONE', #19329, .T. ) ;
#5826 = EDGE_CURVE ( 'NONE', #22315, #2844, #17839, .T. ) ;
#5827 = CARTESIAN_POINT ( 'NONE',  ( -157.5176307659779127, 18.00000000000000355, 60.94675664190624786 ) ) ;
#5828 = EDGE_LOOP ( 'NONE', ( #14901, #9340, #7372, #2902 ) ) ;
#5829 = ORIENTED_EDGE ( 'NONE', *, *, #9811, .F. ) ;
#5830 = CARTESIAN_POINT ( 'NONE',  ( -72.65623182917823897, 87.80665977804258659, 70.23323934248251987 ) ) ;
#5831 = VERTEX_POINT ( 'NONE', #12726 ) ;
#5833 = DIRECTION ( 'NONE',  ( 0.9999164797902015955, 6.965998958219364448E-18, -0.01292414190464157182 ) ) ;
#5832 = CARTESIAN_POINT ( 'NONE',  ( 12.41900304340602368, 188.5914010946799806, 321.5742196380866744 ) ) ;
#5834 = DIRECTION ( 'NONE',  ( -7.125109674381880655E-05, 0.9999848031710253382, -0.005512562950849702291 ) ) ;
#5835 = CARTESIAN_POINT ( 'NONE',  ( -31.27192067738528181, 92.26000739851428989, 81.74748161169398486 ) ) ;
#5836 = ORIENTED_EDGE ( 'NONE', *, *, #27, .F. ) ;
#5837 = CARTESIAN_POINT ( 'NONE',  ( 3.346350515192610064, 70.55846734465492887, -81.07323159506103138 ) ) ;
#5838 = AXIS2_PLACEMENT_3D ( 'NONE', #4659, #3409, #11691 ) ;
#5839 = COLOUR_RGB ( '', 0.66274510, 0.83137255, 0.94901961) ;
#5840 = CARTESIAN_POINT ( 'NONE',  ( -19.00908416305977156, 180.4221386788646271, 76.79453591276953262 ) ) ;
#5841 = EDGE_CURVE ( 'NONE', #22481, #16785, #12846, .T. ) ;
#5842 = VECTOR ( 'NONE', #1274, 1000.000000000000000 ) ;
#5843 = ORIENTED_EDGE ( 'NONE', *, *, #9184, .T. ) ;
#5844 = FACE_OUTER_BOUND ( 'NONE', #8233, .T. ) ;
#5845 = CARTESIAN_POINT ( 'NONE',  ( -89.88240203325172217, 87.91076060644846280, 50.84128159929887403 ) ) ;
#5846 = EDGE_CURVE ( 'NONE', #16236, #18202, #19440, .T. ) ;
#5847 = CARTESIAN_POINT ( 'NONE',  ( 0.000000000000000000, 0.000000000000000000, 0.000000000000000000 ) ) ;
#5848 = ORIENTED_EDGE ( 'NONE', *, *, #4824, .T. ) ;
#5849 = DIRECTION ( 'NONE',  ( 0.8981428216242089979, 0.000000000000000000, 0.4397038457472307593 ) ) ;
#5850 = DIRECTION ( 'NONE',  ( -2.025474946048326158E-22, 1.000000000000000000, -1.876735158486679638E-22 ) ) ;
#5851 = B_SPLINE_CURVE_WITH_KNOTS ( 'NONE', 3,
 ( #21976, #6157, #1113, #16516, #15143, #13416 ),
 .UNSPECIFIED., .F., .F.,
 ( 4, 2, 4 ),
 ( 0.005150358821640622572, 0.006610541308350952570, 0.008070723795061282568 ),
 .UNSPECIFIED. ) ;
#5852 = ORIENTED_EDGE ( 'NONE', *, *, #14970, .T. ) ;
#5853 = DIRECTION ( 'NONE',  ( 0.01292394549866741557, 0.005513023399720776152, 0.9999012842304692006 ) ) ;
#5854 = LINE ( 'NONE', #18176, #15507 ) ;
#5855 = ORIENTED_EDGE ( 'NONE', *, *, #16578, .F. ) ;
#5856 = AXIS2_PLACEMENT_3D ( 'NONE', #202, #9021, #18014 ) ;
#5857 = CARTESIAN_POINT ( 'NONE',  ( 68.30941429790007646, 191.4143309225247549, 255.6230893828509352 ) ) ;
#5858 = PRODUCT ( 'Flange', 'Flange', '', ( #2974 ) ) ;
#5859 = CARTESIAN_POINT ( 'NONE',  ( 87.76353177753586010, 103.0887459898907821, 66.33296338796031932 ) ) ;
#5860 = AXIS2_PLACEMENT_3D ( 'NONE', #4623, #13716, #18640 ) ;
#5861 = CARTESIAN_POINT ( 'NONE',  ( -19.00623411919002592, 140.4227465520235967, 77.01503843080352851 ) ) ;
#5862 = ORIENTED_EDGE ( 'NONE', *, *, #12004, .T. ) ;
#5863 = EDGE_CURVE ( 'NONE', #11287, #6191, #5458, .T. ) ;
#5864 = FACE_OUTER_BOUND ( 'NONE', #14944, .T. ) ;
#5865 = EDGE_LOOP ( 'NONE', ( #3735, #7563, #3487 ) ) ;
#5866 = DIRECTION ( 'NONE',  ( -0.01292414190464077212, 0.000000000000000000, -0.9999164797902015955 ) ) ;
#5867 = DIRECTION ( 'NONE',  ( 1.387778780781444571E-14, 0.000000000000000000, -1.000000000000000000 ) ) ;
#5868 = CARTESIAN_POINT ( 'NONE',  ( 91.21019055468690340, 77.12912189496647386, 28.82359390673205723 ) ) ;
#5869 = DIRECTION ( 'NONE',  ( 0.01292394549866741557, 0.005513023399720270480, 0.9999012842304693116 ) ) ;
#5870 = DIRECTION ( 'NONE',  ( 0.000000000000000000, 0.000000000000000000, 1.000000000000000000 ) ) ;
#5871 = FACE_OUTER_BOUND ( 'NONE', #7023, .T. ) ;
#5872 = DIRECTION ( 'NONE',  ( 0.9999164797902017066, 6.965998958219364448E-18, -0.01292414190464157356 ) ) ;
#5873 = DIRECTION ( 'NONE',  ( 0.000000000000000000, 1.000000000000000000, 0.000000000000000000 ) ) ;
#5874 = ORIENTED_EDGE ( 'NONE', *, *, #21827, .T. ) ;
#5875 = CARTESIAN_POINT ( 'NONE',  ( -64.64710546055418661, 118.1474297122748709, 27.72283698990772649 ) ) ;
#5876 = DIRECTION ( 'NONE',  ( 0.000000000000000000, 1.000000000000000000, -0.000000000000000000 ) ) ;
#5877 = ORIENTED_EDGE ( 'NONE', *, *, #7864, .F. ) ;
#5878 = AXIS2_PLACEMENT_3D ( 'NONE', #16161, #3724, #12706 ) ;
#5879 = EDGE_LOOP ( 'NONE', ( #18124, #7310, #20251, #20130 ) ) ;
#5880 = CARTESIAN_POINT ( 'NONE',  ( -84.94025445842608235, 75.00896870829117802, -0.2173801658002265935 ) ) ;
#5881 = CIRCLE ( 'NONE', #16557, 118.0000000000000000 ) ;
#5882 = CARTESIAN_POINT ( 'NONE',  ( -90.14989025201742834, 88.17731219746620752, 53.00831397183212346 ) ) ;
#5883 = EDGE_CURVE ( 'NONE', #592, #307, #14345, .T. ) ;
#5884 = AXIS2_PLACEMENT_3D ( 'NONE', #21336, #3654, #14245 ) ;
#5885 =( BOUNDED_SURFACE ( )  B_SPLINE_SURFACE ( 3, 2, ( 
 ( #16742, #21520, #15013 ),
 ( #21965, #5788, #6266 ),
 ( #19797, #4072, #18122 ),
 ( #644, #2372, #7631 ),
 ( #21627, #12954, #19918 ),
 ( #4189, #11218, #22423 ),
 ( #10276, #22530, #3249 ),
 ( #17291, #8423, #18991 ),
 ( #20605, #10162, #18658 ),
 ( #3146, #6597, #1553 ) ),
 .UNSPECIFIED., .F., .F., .T. ) 
 B_SPLINE_SURFACE_WITH_KNOTS ( ( 4, 2, 2, 2, 4 ),
 ( 3, 3 ),
 ( 0.5394812760223721693, 0.7973100387155035440, 1.055138801408634919, 1.312967564101766182, 1.570796326794897668 ),
 ( 0.000000000000000000, 1.000000000000000000 ),
 .UNSPECIFIED. ) 
 GEOMETRIC_REPRESENTATION_ITEM ( )  RATIONAL_B_SPLINE_SURFACE ( (
 ( 1.000000000000000000, 0.8430901905886449832, 1.000000000000000000),
 ( 1.000000000000000000, 0.8366591603533565236, 1.000000000000000000),
 ( 1.000000000000000000, 0.8287607763626427815, 1.000000000000000000),
 ( 1.000000000000000000, 0.8103261952457585515, 1.000000000000000000),
 ( 1.000000000000000000, 0.7997876793901601555, 1.000000000000000000),
 ( 1.000000000000000000, 0.7764793049479934428, 1.000000000000000000),
 ( 1.000000000000000000, 0.7637087627022125513, 1.000000000000000000),
 ( 1.000000000000000000, 0.7364885232972262497, 1.000000000000000000),
 ( 1.000000000000000000, 0.7220407509482392738, 1.000000000000000000),
 ( 1.000000000000000000, 0.7071067811865463515, 1.000000000000000000) ) ) 
 REPRESENTATION_ITEM ( '' )  SURFACE ( )  );
#5886 = AXIS2_PLACEMENT_3D ( 'NONE', #11108, #21526, #11444 ) ;
#5887 = ORIENTED_EDGE ( 'NONE', *, *, #14435, .T. ) ;
#5888 = CARTESIAN_POINT ( 'NONE',  ( -38.43592255312495354, 106.3319251612770699, 92.24984488169984331 ) ) ;
#5889 = CIRCLE ( 'NONE', #776, 97.00000000000005684 ) ;
#5890 = PLANE ( 'NONE',  #1900 ) ;
#5891 = CARTESIAN_POINT ( 'NONE',  ( -7.055491003095976765, 165.4026673485312244, 299.7448597359355631 ) ) ;
#5892 = DIRECTION ( 'NONE',  ( -0.9232306267972774094, -1.069144893909151832E-19, 0.3842462878721230046 ) ) ;
#5893 = FACE_OUTER_BOUND ( 'NONE', #1008, .T. ) ;
#5894 = EDGE_CURVE ( 'NONE', #6959, #13713, #8431, .T. ) ;
#5895 = FACE_BOUND ( 'NONE', #14585, .T. ) ;
#5896 = CARTESIAN_POINT ( 'NONE',  ( 73.92355286441096496, 75.01302696078242604, -2.579009233597790107 ) ) ;
#5897 = CARTESIAN_POINT ( 'NONE',  ( 20.06961194383113067, 182.5783991459622655, 314.4765814583797123 ) ) ;
#5898 = CARTESIAN_POINT ( 'NONE',  ( 18.70469657817222853, 88.26328955574699364, -77.54996127225918201 ) ) ;
#5899 = VECTOR ( 'NONE', #8144, 1000.000000000000114 ) ;
#5900 = DIRECTION ( 'NONE',  ( -0.4397038457472424167, 0.000000000000000000, -0.8981428216242032248 ) ) ;
#5901 = EDGE_LOOP ( 'NONE', ( #8869, #7675, #17314, #21480 ) ) ;
#5902 = AXIS2_PLACEMENT_3D ( 'NONE', #7594, #21582, #9886 ) ;
#5903 = CARTESIAN_POINT ( 'NONE',  ( -10.90179587787409865, 113.6756165398083880, 122.8556050573891838 ) ) ;
#5904 = DIRECTION ( 'NONE',  ( -0.9999164797902017066, -2.775557561562891351E-15, 0.01292414190464108437 ) ) ;
#5905 = CIRCLE ( 'NONE', #21654, 3.399999999999985700 ) ;
#5906 = LINE ( 'NONE', #634, #14374 ) ;
#5907 = ORIENTED_EDGE ( 'NONE', *, *, #1645, .F. ) ;
#5908 = DIRECTION ( 'NONE',  ( 0.000000000000000000, 1.000000000000000000, -0.000000000000000000 ) ) ;
#5909 = ORIENTED_EDGE ( 'NONE', *, *, #6115, .F. ) ;
#5910 = ORIENTED_EDGE ( 'NONE', *, *, #11361, .T. ) ;
#5911 = CARTESIAN_POINT ( 'NONE',  ( 42.92324425022518852, 106.8061942917681790, 70.38450200964520320 ) ) ;
#5912 = EDGE_CURVE ( 'NONE', #9437, #17867, #18697, .T. ) ;
#5913 = EDGE_CURVE ( 'NONE', #19030, #20077, #16073, .T. ) ;
#5914 = AXIS2_PLACEMENT_3D ( 'NONE', #1878, #8740, #19214 ) ;
#5915 = AXIS2_PLACEMENT_3D ( 'NONE', #13025, #16465, #1176 ) ;
#5916 = CARTESIAN_POINT ( 'NONE',  ( 75.00823711914057412, 75.00686501439010101, -2.123222951424176941 ) ) ;
#5917 = CARTESIAN_POINT ( 'NONE',  ( -45.96219963993937796, 168.0879242961143518, -74.15276576609245751 ) ) ;
#5918 = AXIS2_PLACEMENT_3D ( 'NONE', #16588, #4257, #9428 ) ;
#5919 = CARTESIAN_POINT ( 'NONE',  ( 74.72480678892256378, 75.05718735177460132, 2.334685081673636198 ) ) ;
#5920 = CARTESIAN_POINT ( 'NONE',  ( 65.90110554552376243, 103.0000000000000000, 69.29678410920483600 ) ) ;
#5921 = VECTOR ( 'NONE', #19563, 1000.000000000000000 ) ;
#5922 = EDGE_LOOP ( 'NONE', ( #22372, #13643, #5471, #9555 ) ) ;
#5923 = DIRECTION ( 'NONE',  ( 1.000000000000000000, 0.000000000000000000, 0.000000000000000000 ) ) ;
#5924 = CARTESIAN_POINT ( 'NONE',  ( 3.238525412985443275, 174.4142081434253555, 256.5568762585190257 ) ) ;
#5925 = CARTESIAN_POINT ( 'NONE',  ( -54.52327687265814404, 1.999999999999998224, 111.3697098814011923 ) ) ;
#5926 = CARTESIAN_POINT ( 'NONE',  ( -8.413499874523651556, 185.3190104300268217, 323.2517229709724234 ) ) ;
#5928 = FACE_OUTER_BOUND ( 'NONE', #225, .T. ) ;
#5927 = CARTESIAN_POINT ( 'NONE',  ( -88.42079784105915508, 80.23159800265108288, 32.23730667790417215 ) ) ;
#5929 = DIRECTION ( 'NONE',  ( -0.01292394549866632963, -0.005513023399716958026, -0.9999012842304692006 ) ) ;
#5930 = VERTEX_POINT ( 'NONE', #1926 ) ;
#5931 = VECTOR ( 'NONE', #16668, 999.9999999999998863 ) ;
#5932 = CARTESIAN_POINT ( 'NONE',  ( 49.20623290202794919, 189.4921571640329603, -92.81436920875947294 ) ) ;
#5933 = STYLED_ITEM ( 'NONE', ( #3962 ), #17112 ) ;
#5934 = ORIENTED_EDGE ( 'NONE', *, *, #3491, .T. ) ;
#5935 = DIRECTION ( 'NONE',  ( -5.440186201345738641E-18, -1.000000000000000000, -1.334940939666364181E-17 ) ) ;
#5936 = CARTESIAN_POINT ( 'NONE',  ( -14.38384282170848572, 181.5288438622440026, 311.2293654625956947 ) ) ;
#5937 = EDGE_LOOP ( 'NONE', ( #16453, #18875, #9271, #15919 ) ) ;
#5938 = AXIS2_PLACEMENT_3D ( 'NONE', #22250, #22356, #6541 ) ;
#5939 = VERTEX_POINT ( 'NONE', #8912 ) ;
#5940 = ADVANCED_FACE ( 'NONE', ( #17904 ), #7198, .F. ) ;
#5941 = PLANE ( 'NONE',  #10624 ) ;
#5942 = CARTESIAN_POINT ( 'NONE',  ( 12.81503532323078964, 190.4972571607467842, 307.8483445055002221 ) ) ;
#5943 = AXIS2_PLACEMENT_3D ( 'NONE', #14675, #13070, #16298 ) ;
#5944 = VECTOR ( 'NONE', #6862, 1000.000000000000227 ) ;
#5945 = AXIS2_PLACEMENT_3D ( 'NONE', #9487, #12964, #775 ) ;
#5946 = DIRECTION ( 'NONE',  ( 1.776356839400250465E-15, 0.000000000000000000, 1.000000000000000000 ) ) ;
#5947 = CARTESIAN_POINT ( 'NONE',  ( -55.30785090598609344, 143.9326556260107282, 169.9740248546933969 ) ) ;
#5948 = VERTEX_POINT ( 'NONE', #3866 ) ;
#5949 = CARTESIAN_POINT ( 'NONE',  ( -64.14977513578709534, 101.1708071963161615, 66.20034608127639331 ) ) ;
#5950 = EDGE_CURVE ( 'NONE', #17515, #15796, #20522, .T. ) ;
#5951 = CARTESIAN_POINT ( 'NONE',  ( -15.09567095940728798, 178.4792087098117577, 317.9922241412446056 ) ) ;
#5952 = ORIENTED_EDGE ( 'NONE', *, *, #21158, .F. ) ;
#5953 = AXIS2_PLACEMENT_3D ( 'NONE', #4681, #7821, #18389 ) ;
#5954 = ORIENTED_EDGE ( 'NONE', *, *, #14587, .F. ) ;
#5955 = FACE_OUTER_BOUND ( 'NONE', #3550, .T. ) ;
#5956 = VERTEX_POINT ( 'NONE', #7885 ) ;
#5957 = CARTESIAN_POINT ( 'NONE',  ( 12.32031054571417705, 188.2809068403609558, 321.9016682987510762 ) ) ;
#5958 = CARTESIAN_POINT ( 'NONE',  ( 8.633533809377718526, 190.8419313418282854, 256.3975693155348381 ) ) ;
#5959 = CARTESIAN_POINT ( 'NONE',  ( -14.25982594500669975, 87.34594711659762822, 76.51465384614120069 ) ) ;
#5960 = ORIENTED_EDGE ( 'NONE', *, *, #14435, .F. ) ;
#5961 = VERTEX_POINT ( 'NONE', #21639 ) ;
#5962 = CARTESIAN_POINT ( 'NONE',  ( 35.95309506732430549, 93.50464841319750064, 82.03286182426640494 ) ) ;
#5963 = AXIS2_PLACEMENT_3D ( 'NONE', #5000, #14221, #77 ) ;
#5964 = AXIS2_PLACEMENT_3D ( 'NONE', #16591, #21812, #6103 ) ;
#5965 = DIRECTION ( 'NONE',  ( 7.125109674364534776E-05, -0.9999848031710252272, 0.005512562950849704893 ) ) ;
#5966 = VERTEX_POINT ( 'NONE', #2605 ) ;
#5967 = ADVANCED_FACE ( 'NONE', ( #20276 ), #18334, .T. ) ;
#5968 = CYLINDRICAL_SURFACE ( 'NONE', #1806, 126.0000000000000000 ) ;
#5969 = CARTESIAN_POINT ( 'NONE',  ( -88.67226694823077082, 88.96335391310392993, 50.75244397949245467 ) ) ;
#5970 = ADVANCED_FACE ( 'NONE', ( #20047 ), #16520, .F. ) ;
#5971 = VECTOR ( 'NONE', #4442, 1000.000000000000227 ) ;
#5972 = DIRECTION ( 'NONE',  ( 0.9820818503191364179, -1.040834085586084257E-17, -0.1884548733085492089 ) ) ;
#5973 = ORIENTED_EDGE ( 'NONE', *, *, #5185, .T. ) ;
#5974 = DIRECTION ( 'NONE',  ( 0.9999164797902017066, 6.965998958219365988E-18, -0.01292414190464157356 ) ) ;
#5975 = CARTESIAN_POINT ( 'NONE',  ( -51.50781950266230069, 111.3281040458452082, -46.57401169717144285 ) ) ;
#5976 = VERTEX_POINT ( 'NONE', #7641 ) ;
#5977 = DIRECTION ( 'NONE',  ( -0.9934404589540163366, -0.1135548637187060866, 0.01346653032743036840 ) ) ;
#5978 = DIRECTION ( 'NONE',  ( 7.125109674161246868E-05, -0.9999848031710253382, 0.005512562950850155054 ) ) ;
#5979 = VECTOR ( 'NONE', #764, 1000.000000000000114 ) ;
#5980 = CARTESIAN_POINT ( 'NONE',  ( -51.99565694909051672, 170.0000000000000284, 0.6720553790413400508 ) ) ;
#5981 = AXIS2_PLACEMENT_3D ( 'NONE', #7005, #22592, #1621 ) ;
#5982 = CYLINDRICAL_SURFACE ( 'NONE', #4186, 2.000000000000004885 ) ;
#5983 = ADVANCED_FACE ( 'NONE', ( #18568 ), #16178, .F. ) ;
#5984 = ORIENTED_EDGE ( 'NONE', *, *, #12021, .F. ) ;
#5985 = CARTESIAN_POINT ( 'NONE',  ( -18.45420839006976621, 164.1078124625656187, 301.8995274031627787 ) ) ;
#5986 = ORIENTED_EDGE ( 'NONE', *, *, #7817, .T. ) ;
#5987 = CARTESIAN_POINT ( 'NONE',  ( -10.91468522650879258, 105.6685712077031241, 121.5997949944007246 ) ) ;
#5988 = ADVANCED_FACE ( 'NONE', ( #11227 ), #326, .T. ) ;
#5989 = CARTESIAN_POINT ( 'NONE',  ( 49.03340997568240311, 189.5897628274961164, -75.10636390159697839 ) ) ;
#5990 = CARTESIAN_POINT ( 'NONE',  ( 17.14168828271968437, 177.4876913356084174, 88.22687136455920154 ) ) ;
#5991 = PLANE ( 'NONE',  #11809 ) ;
#5992 = CARTESIAN_POINT ( 'NONE',  ( 0.000000000000000000, 20.00000000000000000, 0.000000000000000000 ) ) ;
#5993 = EDGE_CURVE ( 'NONE', #1904, #14118, #13607, .T. ) ;
#5994 = EDGE_LOOP ( 'NONE', ( #12687, #3289, #7073, #7551 ) ) ;
#5995 = PLANE ( 'NONE',  #9651 ) ;
#5996 = TOROIDAL_SURFACE ( 'NONE', #18828, 8.000000000000014211, 2.000000000000000000 ) ;
#5997 = CARTESIAN_POINT ( 'NONE',  ( -51.36678610600512940, 111.1441465054529232, -46.50825084614805149 ) ) ;
#5998 = ORIENTED_EDGE ( 'NONE', *, *, #5551, .T. ) ;
#5999 = FACE_OUTER_BOUND ( 'NONE', #19688, .T. ) ;
#6000 = EDGE_LOOP ( 'NONE', ( #18341, #4334, #7973, #5039, #4616, #5960 ) ) ;
#6001 = AXIS2_PLACEMENT_3D ( 'NONE', #12332, #20, #19542 ) ;
#6002 = ADVANCED_FACE ( 'NONE', ( #20493 ), #13850, .F. ) ;
#6003 = AXIS2_PLACEMENT_3D ( 'NONE', #12379, #17435, #19358 ) ;
#6004 = CARTESIAN_POINT ( 'NONE',  ( -84.97839964729169537, 75.00686501439008680, -0.05536024668152433881 ) ) ;
#6005 = CARTESIAN_POINT ( 'NONE',  ( -90.14962381271330116, 88.05998628382424442, 53.08008600111026709 ) ) ;
#6006 = ADVANCED_FACE ( 'NONE', ( #17422 ), #22434, .F. ) ;
#6007 = ADVANCED_FACE ( 'NONE', ( #13748 ), #13417, .T. ) ;
#6008 = ORIENTED_EDGE ( 'NONE', *, *, #2760, .F. ) ;
#6009 = ORIENTED_EDGE ( 'NONE', *, *, #14081, .F. ) ;
#6010 = CARTESIAN_POINT ( 'NONE',  ( 14.14224087380716455, 105.6999953372425409, 126.9762993157022777 ) ) ;
#6011 = DIRECTION ( 'NONE',  ( 0.01292414190464131335, 1.902755938799530239E-22, 0.9999164797902015955 ) ) ;
#6012 = VECTOR ( 'NONE', #12777, 1000.000000000000114 ) ;
#6013 = AXIS2_PLACEMENT_3D ( 'NONE', #20888, #17354, #2059 ) ;
#6014 = CARTESIAN_POINT ( 'NONE',  ( -37.14537067542799065, 95.89621381637979880, 85.13594009840959131 ) ) ;
#6015 = ORIENTED_EDGE ( 'NONE', *, *, #2503, .T. ) ;
#6016 = CARTESIAN_POINT ( 'NONE',  ( -44.99638338670928306, 229.0513208305363548, 372.9597790112123334 ) ) ;
#6017 = LINE ( 'NONE', #11417, #8917 ) ;
#6018 = CARTESIAN_POINT ( 'NONE',  ( 20.00631865610750637, 182.6246599348329767, 313.5209380637898562 ) ) ;
#6019 = TOROIDAL_SURFACE ( 'NONE', #19581, 77.00000000000002842, 2.000000000000000000 ) ;
#6020 = CARTESIAN_POINT ( 'NONE',  ( 14.26922013821070934, 87.34719917405588774, -76.51617212798838352 ) ) ;
#6021 = AXIS2_PLACEMENT_3D ( 'NONE', #10738, #15584, #12242 ) ;
#6022 = PLANE ( 'NONE',  #18368 ) ;
#6023 = EDGE_CURVE ( 'NONE', #4506, #5956, #20833, .T. ) ;
#6024 = ORIENTED_EDGE ( 'NONE', *, *, #6810, .T. ) ;
#6025 =( NAMED_UNIT ( * ) SI_UNIT ( $, .STERADIAN. ) SOLID_ANGLE_UNIT ( ) );
#6026 = CARTESIAN_POINT ( 'NONE',  ( 51.71043826665287924, 166.8507685304810764, 255.9730676870379114 ) ) ;
#6027 = CARTESIAN_POINT ( 'NONE',  ( -49.64992578782946708, 140.1470953820375200, 27.40769847641928791 ) ) ;
#6028 = ORIENTED_EDGE ( 'NONE', *, *, #7366, .T. ) ;
#6029 = VECTOR ( 'NONE', #19401, 1000.000000000000227 ) ;
#6030 = DIRECTION ( 'NONE',  ( -0.000000000000000000, -1.000000000000000000, -0.000000000000000000 ) ) ;
#6031 = ORIENTED_EDGE ( 'NONE', *, *, #12663, .T. ) ;
#6032 = ORIENTED_EDGE ( 'NONE', *, *, #3400, .F. ) ;
#6033 = CARTESIAN_POINT ( 'NONE',  ( 64.31463902574824942, 189.7102623349351802, -53.44513790491837568 ) ) ;
#6034 = CARTESIAN_POINT ( 'NONE',  ( -23.44527677710862434, -5.346239964818074952, -10.02852836536016845 ) ) ;
#6035 = ADVANCED_FACE ( 'NONE', ( #19116 ), #6247, .F. ) ;
#6036 = VECTOR ( 'NONE', #15260, 1000.000000000000114 ) ;
#6037 = AXIS2_PLACEMENT_3D ( 'NONE', #19101, #22625, #22299 ) ;
#6038 = CARTESIAN_POINT ( 'NONE',  ( 14.14167086503323034, 113.6998737626107641, 126.9321988120954643 ) ) ;
#6039 = CARTESIAN_POINT ( 'NONE',  ( 75.97949114995992659, 75.05057272691708192, 2.129988415395909218 ) ) ;
#6040 = DIRECTION ( 'NONE',  ( 0.01292394549866741557, 0.005513023399720270480, 0.9999012842304693116 ) ) ;
#6041 = CARTESIAN_POINT ( 'NONE',  ( 12.08460136693709153, 159.1320474315246543, 323.5344127036669875 ) ) ;
#6042 = CARTESIAN_POINT ( 'NONE',  ( 26.25061226286096883, 169.2177813299073819, 301.2935335384283917 ) ) ;
#6043 = B_SPLINE_CURVE_WITH_KNOTS ( 'NONE', 3,
 ( #18696, #21814, #17968, #13132, #4260, #14873, #5997, #5651, #2203, #16593, #4031, #610, #21378, #11283 ),
 .UNSPECIFIED., .F., .F.,
 ( 4, 2, 2, 2, 2, 2, 4 ),
 ( 0.000000000000000000, 0.0005796598520817377968, 0.001159319704163475594, 0.001738979556245213174, 0.002318639408326951187, 0.003477959112490424613, 0.004637278816653898905 ),
 .UNSPECIFIED. ) ;
#6044 = ORIENTED_EDGE ( 'NONE', *, *, #14479, .F. ) ;
#6045 = CARTESIAN_POINT ( 'NONE',  ( -10.85595612533484911, 109.6999345499266525, 127.2773526115149281 ) ) ;
#6046 = ORIENTED_EDGE ( 'NONE', *, *, #4686, .F. ) ;
#6047 = DIRECTION ( 'NONE',  ( 0.9996018883047153025, 0.0001555065151365095106, 0.02821419350913914950 ) ) ;
#6048 = AXIS2_PLACEMENT_3D ( 'NONE', #13497, #11764, #20589 ) ;
#6049 = CARTESIAN_POINT ( 'NONE',  ( -56.88925295215435085, 118.2576901802692646, 47.62393161023230448 ) ) ;
#6050 = CARTESIAN_POINT ( 'NONE',  ( -19.99832959580404790, 170.0000000000008242, 0.2584828380936761705 ) ) ;
#6051 = CARTESIAN_POINT ( 'NONE',  ( -70.91392079944854743, 69.99999999999998579, -84.09052168258642723 ) ) ;
#6052 = ADVANCED_FACE ( 'NONE', ( #4873 ), #8433, .F. ) ;
#6053 = ADVANCED_FACE ( 'NONE', ( #15261 ), #19001, .F. ) ;
#6054 = DIRECTION ( 'NONE',  ( 0.01292414190464131335, 0.000000000000000000, 0.9999164797902017066 ) ) ;
#6055 = ORIENTED_EDGE ( 'NONE', *, *, #14323, .T. ) ;
#6056 = DIRECTION ( 'NONE',  ( 0.01292394549866738955, 0.005513023399720468239, 0.9999012842304693116 ) ) ;
#6057 = CARTESIAN_POINT ( 'NONE',  ( -7.930164461608248607E-16, 20.00000000000000000, -7.999999999999994671 ) ) ;
#6058 = CARTESIAN_POINT ( 'NONE',  ( -9.227205039120967456, 184.9256890989761644, 305.2585128821986018 ) ) ;
#6059 = ORIENTED_EDGE ( 'NONE', *, *, #13849, .T. ) ;
#6060 = ORIENTED_EDGE ( 'NONE', *, *, #18021, .T. ) ;
#6061 = LINE ( 'NONE', #2397, #20514 ) ;
#6062 = CIRCLE ( 'NONE', #7897, 110.5324305509042233 ) ;
#6063 = CARTESIAN_POINT ( 'NONE',  ( -109.3418654547023721, 87.00751446224754204, 51.62948579205222899 ) ) ;
#6064 = DIRECTION ( 'NONE',  ( 0.01292394549866743812, 0.005513023399720639109, 0.9999012842304693116 ) ) ;
#6065 = LINE ( 'NONE', #2507, #5971 ) ;
#6066 = EDGE_LOOP ( 'NONE', ( #17206, #11430, #22627, #3829 ) ) ;
#6067 = CARTESIAN_POINT ( 'NONE',  ( -63.91983116576977153, 91.51644034066822542, 67.07156771589210109 ) ) ;
#6068 = CARTESIAN_POINT ( 'NONE',  ( -13.49256607648177209, 180.7387789766418962, 321.2375318158862001 ) ) ;
#6069 = EDGE_CURVE ( 'NONE', #8492, #22201, #821, .T. ) ;
#6070 = EDGE_LOOP ( 'NONE', ( #7754, #21406, #1972, #15939 ) ) ;
#6071 = ORIENTED_EDGE ( 'NONE', *, *, #15423, .F. ) ;
#6072 = CARTESIAN_POINT ( 'NONE',  ( -101.0000000000000000, 29.00000000000000355, 0.000000000000000000 ) ) ;
#6073 = LINE ( 'NONE', #15048, #909 ) ;
#6074 = VECTOR ( 'NONE', #1642, 1000.000000000000000 ) ;
#6075 = CARTESIAN_POINT ( 'NONE',  ( -42.28414214406363669, 95.00650440594678514, -43.52932268794753412 ) ) ;
#6076 = CARTESIAN_POINT ( 'NONE',  ( 13.24479188061246759, 86.89994116914630240, 75.66937141396037703 ) ) ;
#6077 = ORIENTED_EDGE ( 'NONE', *, *, #7562, .T. ) ;
#6078 = ORIENTED_EDGE ( 'NONE', *, *, #17151, .F. ) ;
#6079 = CARTESIAN_POINT ( 'NONE',  ( -2.096375399687118168, 190.2200455327031534, 274.6112675210154634 ) ) ;
#6080 = CARTESIAN_POINT ( 'NONE',  ( -8.628845071887251805, 185.6862342536340691, 306.4543981107967738 ) ) ;
#6081 = ORIENTED_EDGE ( 'NONE', *, *, #10213, .F. ) ;
#6082 = CARTESIAN_POINT ( 'NONE',  ( 12.39776786404130782, 161.0697644098447370, 324.5197799491688215 ) ) ;
#6083 = CARTESIAN_POINT ( 'NONE',  ( -88.17149547474421922, 88.83987025360480061, 52.15764617096433398 ) ) ;
#6084 = AXIS2_PLACEMENT_3D ( 'NONE', #15414, #12409, #10672 ) ;
#6085 = VERTEX_POINT ( 'NONE', #8655 ) ;
#6086 = FACE_OUTER_BOUND ( 'NONE', #12984, .T. ) ;
#6087 = CARTESIAN_POINT ( 'NONE',  ( -51.98136777917161311, 109.9521095004071753, -43.50144448901883720 ) ) ;
#6088 = CARTESIAN_POINT ( 'NONE',  ( 13.81123123916535356, 189.8530796209156790, 320.7501109915356210 ) ) ;
#6089 = FACE_OUTER_BOUND ( 'NONE', #10271, .T. ) ;
#6090 = DIRECTION ( 'NONE',  ( 0.3834992599886433706, -0.005063754594578209756, -0.9235273011544211652 ) ) ;
#6091 = ORIENTED_EDGE ( 'NONE', *, *, #3164, .T. ) ;
#6092 = DIRECTION ( 'NONE',  ( -0.7562662552911934011, -0.5735764363510515995, 0.3147561322209046497 ) ) ;
#6093 = DIRECTION ( 'NONE',  ( 0.01292394549866733230, 0.005513023399720419666, 0.9999012842304692006 ) ) ;
#6094 = CARTESIAN_POINT ( 'NONE',  ( 68.71681667565952978, 91.32006346413032816, -85.89527988174788220 ) ) ;
#6095 = ORIENTED_EDGE ( 'NONE', *, *, #19326, .F. ) ;
#6096 = CARTESIAN_POINT ( 'NONE',  ( 37.83293359763302988, 93.41702043944185618, -84.07896005542636431 ) ) ;
#6097 = ORIENTED_EDGE ( 'NONE', *, *, #21966, .F. ) ;
#6098 = DIRECTION ( 'NONE',  ( -0.007371307436792093500, 0.7031977520565657613, -0.7109561064716055645 ) ) ;
#6099 = CARTESIAN_POINT ( 'NONE',  ( -109.6289368035921683, 77.12912189496647386, 29.41931704363643618 ) ) ;
#6100 = CARTESIAN_POINT ( 'NONE',  ( 0.000000000000000000, 1.999999999999998224, 0.000000000000000000 ) ) ;
#6101 = PLANE ( 'NONE',  #5918 ) ;
#6102 = ADVANCED_FACE ( 'NONE', ( #20385 ), #4646, .F. ) ;
#6103 = DIRECTION ( 'NONE',  ( 1.386679829960243061E-14, 0.000000000000000000, 1.000000000000000000 ) ) ;
#6104 = DIRECTION ( 'NONE',  ( -0.7480173694308205334, 0.4911576187806371285, 0.4463565934805150959 ) ) ;
#6105 = DIRECTION ( 'NONE',  ( 2.025474946048326158E-22, -1.000000000000000000, 1.876735158486679638E-22 ) ) ;
#6106 = ORIENTED_EDGE ( 'NONE', *, *, #6858, .F. ) ;
#6107 = LINE ( 'NONE', #18194, #10200 ) ;
#6108 = ADVANCED_BREP_SHAPE_REPRESENTATION ( '', ( #2374, #6292 ), #21305 ) ;
#6109 = ORIENTED_EDGE ( 'NONE', *, *, #6225, .F. ) ;
#6110 = ORIENTED_EDGE ( 'NONE', *, *, #13658, .F. ) ;
#6111 = CARTESIAN_POINT ( 'NONE',  ( -83.41629690720331780, 75.07731437015503673, -2.761324039041341827 ) ) ;
#6112 = EDGE_CURVE ( 'NONE', #19328, #6852, #15357, .T. ) ;
#6113 = CARTESIAN_POINT ( 'NONE',  ( -88.16190907930861442, 88.08529935286561852, 53.04065179493614579 ) ) ;
#6114 = ADVANCED_FACE ( 'NONE', ( #19573 ), #12367, .T. ) ;
#6115 = EDGE_CURVE ( 'NONE', #9640, #3676, #1482, .T. ) ;
#6117 = VERTEX_POINT ( 'NONE', #14441 ) ;
#6116 = ORIENTED_EDGE ( 'NONE', *, *, #1695, .F. ) ;
#6118 = EDGE_CURVE ( 'NONE', #198, #11245, #20539, .T. ) ;
#6119 = CYLINDRICAL_SURFACE ( 'NONE', #4458, 10.00000000000000888 ) ;
#6120 = CARTESIAN_POINT ( 'NONE',  ( -90.00000000000000000, 45.00100000000000477, -10.99999999999999289 ) ) ;
#6121 = CARTESIAN_POINT ( 'NONE',  ( -93.17671387018313567, 79.04398536104955042, -26.22064129356660800 ) ) ;
#6122 = CARTESIAN_POINT ( 'NONE',  ( 70.78416300399058514, 71.33159407511109862, 84.19980244608490239 ) ) ;
#6123 = VERTEX_POINT ( 'NONE', #20952 ) ;
#6124 = AXIS2_PLACEMENT_3D ( 'NONE', #14744, #4248, #11270 ) ;
#6125 = ORIENTED_EDGE ( 'NONE', *, *, #21705, .F. ) ;
#6126 = CARTESIAN_POINT ( 'NONE',  ( -48.94038278341281512, 95.51270090492249665, 82.30370228625183415 ) ) ;
#6127 = DIRECTION ( 'NONE',  ( -0.01292394549866738782, -0.005513023399720700692, -0.9999012842304693116 ) ) ;
#6128 = CARTESIAN_POINT ( 'NONE',  ( 18.54778899613519982, 185.5359755103985719, 318.0241678234317533 ) ) ;
#6129 = CARTESIAN_POINT ( 'NONE',  ( 11.27395757585026637, 86.89847835976068779, -75.98467626014961240 ) ) ;
#6130 = EDGE_CURVE ( 'NONE', #6788, #13046, #17642, .T. ) ;
#6131 = EDGE_CURVE ( 'NONE', #3408, #14037, #8891, .T. ) ;
#6132 = CARTESIAN_POINT ( 'NONE',  ( 146.4999999999998579, 20.00000000000000000, 9.999999999997978506 ) ) ;
#6133 = ORIENTED_EDGE ( 'NONE', *, *, #20759, .F. ) ;
#6134 = SHAPE_REPRESENTATION_RELATIONSHIP ( 'NONE' , 'NONE' ,  #17373, #14307 ) ;
#6135 = CARTESIAN_POINT ( 'NONE',  ( 91.10494378670944116, 97.90071567704912070, 61.64404307423180995 ) ) ;
#6136 = EDGE_CURVE ( 'NONE', #17033, #4427, #14208, .T. ) ;
#6137 = CARTESIAN_POINT ( 'NONE',  ( 55.40268456415105902, 18.00000000000000355, -113.1659955246503699 ) ) ;
#6138 = CARTESIAN_POINT ( 'NONE',  ( -2.098214363056787768, 157.4140274948258593, 299.7248317441846552 ) ) ;
#6139 = ORIENTED_EDGE ( 'NONE', *, *, #12847, .F. ) ;
#6140 = DIRECTION ( 'NONE',  ( -2.459148776294495979E-24, 1.000000000000000000, -1.902597020224326827E-22 ) ) ;
#6141 = VERTEX_POINT ( 'NONE', #19233 ) ;
#6142 = CARTESIAN_POINT ( 'NONE',  ( -162.0000000000000000, 0.000000000000000000, 8.000000000000019540 ) ) ;
#6143 = VECTOR ( 'NONE', #13600, 1000.000000000000000 ) ;
#6144 = EDGE_CURVE ( 'NONE', #11245, #11382, #19347, .T. ) ;
#6145 = CARTESIAN_POINT ( 'NONE',  ( -3.719543892204659752, 174.4361193905359642, 323.6543047440632108 ) ) ;
#6146 = ADVANCED_FACE ( 'NONE', ( #10963 ), #10286, .F. ) ;
#6147 = ORIENTED_EDGE ( 'NONE', *, *, #19504, .T. ) ;
#6148 = EDGE_CURVE ( 'NONE', #1989, #13001, #1848, .T. ) ;
#6149 = CARTESIAN_POINT ( 'NONE',  ( 19.46746992363642903, 137.6261247937603969, 113.4190577045456223 ) ) ;
#6150 = FACE_OUTER_BOUND ( 'NONE', #17976, .T. ) ;
#6151 = DIRECTION ( 'NONE',  ( 7.125109674160325297E-05, -0.9999848031710253382, 0.005512562950849327591 ) ) ;
#6152 = CARTESIAN_POINT ( 'NONE',  ( -40.65297087429915024, 172.4862325201987403, 269.1369983955533485 ) ) ;
#6153 = ORIENTED_EDGE ( 'NONE', *, *, #9991, .F. ) ;
#6154 = CARTESIAN_POINT ( 'NONE',  ( -44.07569325658431580, 153.9910965579657613, 275.2838043771024559 ) ) ;
#6155 = CARTESIAN_POINT ( 'NONE',  ( 2.326345542835435154, 0.000000000000000000, 179.9849663622363778 ) ) ;
#6156 = DIRECTION ( 'NONE',  ( 0.01292394549866738782, 0.005513023399720468239, 0.9999012842304692006 ) ) ;
#6157 = CARTESIAN_POINT ( 'NONE',  ( -52.29297186722168078, 114.5561862689215928, 172.2806101653237079 ) ) ;
#6158 = CIRCLE ( 'NONE', #18986, 4.999999999999990230 ) ;
#6159 = ADVANCED_FACE ( 'NONE', ( #7060 ), #8801, .F. ) ;
#6160 = CARTESIAN_POINT ( 'NONE',  ( 90.41664810497508142, 79.20851322806770156, -29.13399567714613525 ) ) ;
#6161 = CARTESIAN_POINT ( 'NONE',  ( -8.391866834692953248, 185.3333697219060809, 323.2521960560945331 ) ) ;
#6162 = DIRECTION ( 'NONE',  ( 0.01292414190464270286, 1.902755938799533530E-22, 0.9999164797902017066 ) ) ;
#6163 = ORIENTED_EDGE ( 'NONE', *, *, #16295, .F. ) ;
#6164 = CARTESIAN_POINT ( 'NONE',  ( 48.61019632265355028, 162.7612900215456762, 276.0376611274493257 ) ) ;
#6165 = ORIENTED_EDGE ( 'NONE', *, *, #11816, .F. ) ;
#6166 = EDGE_LOOP ( 'NONE', ( #6328, #1798, #382, #22076, #1661, #21171 ) ) ;
#6167 = FACE_OUTER_BOUND ( 'NONE', #16034, .T. ) ;
#6168 = CARTESIAN_POINT ( 'NONE',  ( -10.47940244875819538, 187.4174437848855348, 308.2255844705966297 ) ) ;
#6169 = ORIENTED_EDGE ( 'NONE', *, *, #12819, .F. ) ;
#6170 = VECTOR ( 'NONE', #8237, 1000.000000000000000 ) ;
#6171 = ORIENTED_EDGE ( 'NONE', *, *, #1658, .F. ) ;
#6172 = AXIS2_PLACEMENT_3D ( 'NONE', #643, #16634, #11100 ) ;
#6173 = APPLICATION_CONTEXT ( 'automotive_design' ) ;
#6174 = DIRECTION ( 'NONE',  ( -0.000000000000000000, -1.000000000000000000, -0.000000000000000000 ) ) ;
#6175 = EDGE_CURVE ( 'NONE', #21849, #10639, #2445, .T. ) ;
#6176 = DIRECTION ( 'NONE',  ( 7.125109674161246868E-05, -0.9999848031710252272, 0.005512562950850154186 ) ) ;
#6177 = CARTESIAN_POINT ( 'NONE',  ( -5.731715098087014404, 326.6288426432528240, 307.3396573775339107 ) ) ;
#6178 = AXIS2_PLACEMENT_3D ( 'NONE', #4614, #14987, #11531 ) ;
#6179 = ORIENTED_EDGE ( 'NONE', *, *, #16567, .T. ) ;
#6180 = PLANE ( 'NONE',  #22243 ) ;
#6181 = ADVANCED_FACE ( 'NONE', ( #5557 ), #12589, .F. ) ;
#6182 = CARTESIAN_POINT ( 'NONE',  ( -14.60065500149918805, 179.2330876351038285, 319.3326537707700936 ) ) ;
#6183 = ORIENTED_EDGE ( 'NONE', *, *, #9948, .T. ) ;
#6184 = CARTESIAN_POINT ( 'NONE',  ( -106.6839260360359987, 79.12661604778574542, -26.80604816241528709 ) ) ;
#6185 = COLOUR_RGB ( '', 0.72549020, 0.75294118, 0.79215686) ;
#6186 = CARTESIAN_POINT ( 'NONE',  ( 105.6473595942261738, 69.99999999999998579, 30.63715735456338862 ) ) ;
#6187 = DIRECTION ( 'NONE',  ( -2.025474946048326158E-22, 1.000000000000000000, -1.876735158486679638E-22 ) ) ;
#6188 = ORIENTED_EDGE ( 'NONE', *, *, #13431, .T. ) ;
#6189 = CARTESIAN_POINT ( 'NONE',  ( -55.33894950108811628, 126.9191314136040063, 167.5679852142817197 ) ) ;
#6190 = DIRECTION ( 'NONE',  ( 7.125109674364534776E-05, -0.9999848031710252272, 0.005512562950849704893 ) ) ;
#6191 = VERTEX_POINT ( 'NONE', #871 ) ;
#6192 = AXIS2_PLACEMENT_3D ( 'NONE', #22021, #6326, #13345 ) ;
#6193 = DIRECTION ( 'NONE',  ( -0.01292394549866731843, -0.005513023399720594006, -0.9999012842304693116 ) ) ;
#6194 = CARTESIAN_POINT ( 'NONE',  ( -88.17226140160809678, 88.87231815780248212, 52.07896878194610935 ) ) ;
#6195 = EDGE_CURVE ( 'NONE', #18453, #4632, #14999, .T. ) ;
#6196 = EDGE_CURVE ( 'NONE', #8063, #20449, #1128, .T. ) ;
#6197 = CIRCLE ( 'NONE', #14672, 4.200000000000005507 ) ;
#6199 = ORIENTED_EDGE ( 'NONE', *, *, #7835, .T. ) ;
#6198 = ORIENTED_EDGE ( 'NONE', *, *, #7756, .T. ) ;
#6200 = CARTESIAN_POINT ( 'NONE',  ( -51.49911578223353814, 109.7083498255462075, -43.50633371739562705 ) ) ;
#6201 = CARTESIAN_POINT ( 'NONE',  ( 15.39737658676448895, 188.8107569276171773, 320.3072530890422627 ) ) ;
#6202 = DIRECTION ( 'NONE',  ( -0.01292394549866739996, -0.005513023399721131770, -0.9999012842304692006 ) ) ;
#6203 = DIRECTION ( 'NONE',  ( 0.000000000000000000, 1.000000000000000000, -0.000000000000000000 ) ) ;
#6204 = ORIENTED_EDGE ( 'NONE', *, *, #21833, .F. ) ;
#6205 = FACE_OUTER_BOUND ( 'NONE', #19394, .T. ) ;
#6206 = CARTESIAN_POINT ( 'NONE',  ( 3.545303425248413465, 70.63018678438872655, -91.95213924926606808 ) ) ;
#6207 = CARTESIAN_POINT ( 'NONE',  ( 64.31563894222803413, 189.7102623349352086, -53.44515082906027459 ) ) ;
#6208 = ORIENTED_EDGE ( 'NONE', *, *, #16740, .T. ) ;
#6209 = CARTESIAN_POINT ( 'NONE',  ( -38.68617183816869698, 163.9153776386440882, 273.1592279730091377 ) ) ;
#6210 = EDGE_LOOP ( 'NONE', ( #14831, #4562, #16614, #2850 ) ) ;
#6211 = LINE ( 'NONE', #18514, #6640 ) ;
#6212 = CLOSED_SHELL ( 'NONE', ( #11995, #1634, #21656, #12256, #1822, #21563, #18897, #18492, #21796, #21789, #21879, #21815, #4884, #3064, #21276, #8373, #21868, #17240, #18245, #13908, #6795, #975, #10243, #17114, #15901, #13979, #4089, #4967, #1001, #18360, #21420, #5624, #17444, #19324 ) ) ;
#6213 = CARTESIAN_POINT ( 'NONE',  ( 84.78539177974978713, 105.0000000000000000, 70.08164767436862519 ) ) ;
#6214 = CARTESIAN_POINT ( 'NONE',  ( -9.322685960893931423, 145.0715325292690920, 276.3947491604697007 ) ) ;
#6215 = LINE ( 'NONE', #21810, #9604 ) ;
#6216 = CIRCLE ( 'NONE', #3263, 24.99999999999998224 ) ;
#6217 = PRODUCT_RELATED_PRODUCT_CATEGORY ( 'part', '', ( #14902 ) ) ;
#6218 = CARTESIAN_POINT ( 'NONE',  ( -64.99457118636313169, 170.0000000000000284, 0.8400692238016805868 ) ) ;
#6219 = FACE_OUTER_BOUND ( 'NONE', #11180, .T. ) ;
#6220 = VECTOR ( 'NONE', #18928, 999.9999999999998863 ) ;
#6221 = EDGE_LOOP ( 'NONE', ( #14252, #14224, #13123, #7707 ) ) ;
#6222 = CARTESIAN_POINT ( 'NONE',  ( -55.30785090598609344, 143.9326556260107282, 169.9740248546933685 ) ) ;
#6223 = ORIENTED_EDGE ( 'NONE', *, *, #19213, .F. ) ;
#6224 =( NAMED_UNIT ( * ) SI_UNIT ( $, .STERADIAN. ) SOLID_ANGLE_UNIT ( ) );
#6225 = EDGE_CURVE ( 'NONE', #5690, #19747, #7863, .T. ) ;
#6226 = CARTESIAN_POINT ( 'NONE',  ( -88.16157026904535599, 88.04290212818546024, 53.06700061362209908 ) ) ;
#6227 = CARTESIAN_POINT ( 'NONE',  ( -36.79710281205949940, 121.2962013336460956, 248.0606072992719930 ) ) ;
#6228 = VECTOR ( 'NONE', #11012, 1000.000000000000114 ) ;
#6230 = ORIENTED_EDGE ( 'NONE', *, *, #8774, .F. ) ;
#6229 = ORIENTED_EDGE ( 'NONE', *, *, #9098, .F. ) ;
#6231 = TOROIDAL_SURFACE ( 'NONE', #2188, -102.0000000000000000, 120.0000000000000000 ) ;
#6232 = VECTOR ( 'NONE', #4118, 1000.000000000000227 ) ;
#6233 = DIRECTION ( 'NONE',  ( -0.000000000000000000, -1.000000000000000000, -0.000000000000000000 ) ) ;
#6234 = LINE ( 'NONE', #6120, #22302 ) ;
#6235 = ORIENTED_EDGE ( 'NONE', *, *, #16847, .F. ) ;
#6236 = LINE ( 'NONE', #13261, #9636 ) ;
#6237 = DIRECTION ( 'NONE',  ( 0.9999164797902015955, 0.000000000000000000, -0.01292414190464118845 ) ) ;
#6238 = CARTESIAN_POINT ( 'NONE',  ( -88.41758806590422637, 80.31838830481380853, 32.48564084813592956 ) ) ;
#6239 = CARTESIAN_POINT ( 'NONE',  ( 70.88639693877763648, 71.65513756697318115, 84.11375151051876742 ) ) ;
#6240 = AXIS2_PLACEMENT_3D ( 'NONE', #20523, #4785, #19031 ) ;
#6241 = ORIENTED_EDGE ( 'NONE', *, *, #14703, .T. ) ;
#6242 = CARTESIAN_POINT ( 'NONE',  ( 9.260057161142448479, 190.1982426752826143, 274.6915518483514234 ) ) ;
#6243 = CARTESIAN_POINT ( 'NONE',  ( 19.73688183432247811, 182.9419304313151429, 316.3130507777162279 ) ) ;
#6244 = DIRECTION ( 'NONE',  ( 0.9726991065672921932, 0.2316562896908778701, -0.01384960395994898168 ) ) ;
#6245 = EDGE_CURVE ( 'NONE', #13213, #15391, #6246, .T. ) ;
#6246 = LINE ( 'NONE', #20250, #11018 ) ;
#6247 = TOROIDAL_SURFACE ( 'NONE', #5126, 83.00000000000001421, 2.000000000000000000 ) ;
#6248 = PRODUCT_DEFINITION_SHAPE ( 'NONE', 'NONE',  #18701 ) ;
#6249 = CIRCLE ( 'NONE', #7337, 95.00000000000004263 ) ;
#6250 = CARTESIAN_POINT ( 'NONE',  ( -39.42082737383935154, 72.00000000000000000, 83.51645567887779009 ) ) ;
#6251 = CARTESIAN_POINT ( 'NONE',  ( -91.23603883849614249, 78.43035437438885538, -30.82342686631250217 ) ) ;
#6252 = VERTEX_POINT ( 'NONE', #7521 ) ;
#6253 = AXIS2_PLACEMENT_3D ( 'NONE', #21752, #19925, #21636 ) ;
#6254 = FACE_OUTER_BOUND ( 'NONE', #14047, .T. ) ;
#6255 = ORIENTED_EDGE ( 'NONE', *, *, #3114, .T. ) ;
#6256 = ORIENTED_EDGE ( 'NONE', *, *, #14980, .F. ) ;
#6257 = CARTESIAN_POINT ( 'NONE',  ( 47.76156380321228312, 110.4315385716095079, -44.79328732961231907 ) ) ;
#6258 = CARTESIAN_POINT ( 'NONE',  ( 41.91771097984041461, 107.0053247559779805, 70.57445437474680716 ) ) ;
#6259 = VECTOR ( 'NONE', #17992, 999.9999999999998863 ) ;
#6260 = VERTEX_POINT ( 'NONE', #2461 ) ;
#6261 = EDGE_CURVE ( 'NONE', #9056, #21621, #15457, .T. ) ;
#6262 = EDGE_LOOP ( 'NONE', ( #19835, #11435, #16456, #17358 ) ) ;
#6263 = EDGE_CURVE ( 'NONE', #11245, #2836, #762, .T. ) ;
#6264 = DIRECTION ( 'NONE',  ( 0.01292394549866738261, 0.005513023399722618428, 0.9999012842304692006 ) ) ;
#6265 = CARTESIAN_POINT ( 'NONE',  ( 76.82405103886378583, 75.08619966718657679, -5.043654882722200306 ) ) ;
#6266 = CARTESIAN_POINT ( 'NONE',  ( -90.86534537526709698, 70.37233884329080524, 61.70249327685399976 ) ) ;
#6267 = VECTOR ( 'NONE', #17063, 1000.000000000000227 ) ;
#6268 = CARTESIAN_POINT ( 'NONE',  ( 84.75118562858013149, 75.08956945039734876, 3.039329696154879024 ) ) ;
#6269 = AXIS2_PLACEMENT_3D ( 'NONE', #20101, #10942, #2967 ) ;
#6270 = CARTESIAN_POINT ( 'NONE',  ( 12.84378735233264379, 190.4863133572641232, 307.8501959441126701 ) ) ;
#6271 = CIRCLE ( 'NONE', #2599, 110.5324305509042233 ) ;
#6272 = EDGE_LOOP ( 'NONE', ( #21034, #13219, #16625, #15937 ) ) ;
#6273 = CARTESIAN_POINT ( 'NONE',  ( -1.163172771417702700, 70.63018678438872655, -89.99248318111824574 ) ) ;
#6274 = VERTEX_POINT ( 'NONE', #7962 ) ;
#6275 = CARTESIAN_POINT ( 'NONE',  ( 64.05894960112136971, 189.6011917897851333, -73.22734637019877368 ) ) ;
#6276 = CARTESIAN_POINT ( 'NONE',  ( 90.02055463237803679, 95.44063823554751025, -63.21629334023821656 ) ) ;
#6277 = CARTESIAN_POINT ( 'NONE',  ( -4.505147608247620283, 176.8666157021447134, 324.6511568656583222 ) ) ;
#6278 = EDGE_CURVE ( 'NONE', #19256, #17288, #12125, .T. ) ;
#6279 = CARTESIAN_POINT ( 'NONE',  ( 90.99469209931193348, 80.00980328568967082, -31.64094806796699544 ) ) ;
#6280 = AXIS2_PLACEMENT_3D ( 'NONE', #16623, #21736, #874 ) ;
#6281 = ADVANCED_FACE ( 'NONE', ( #4391 ), #14663, .T. ) ;
#6282 = DIRECTION ( 'NONE',  ( 0.01125613334114014194, 0.4913919529878064685, 0.8708658036695641202 ) ) ;
#6283 = ORIENTED_EDGE ( 'NONE', *, *, #19767, .T. ) ;
#6284 = CARTESIAN_POINT ( 'NONE',  ( 51.60019979106836985, 180.9901659820745294, 273.9681169626219344 ) ) ;
#6285 = ADVANCED_FACE ( 'NONE', ( #522 ), #20122, .F. ) ;
#6286 = VERTEX_POINT ( 'NONE', #21948 ) ;
#6287 = CARTESIAN_POINT ( 'NONE',  ( -2.067862704742604141, 72.00000000000000000, -159.9866367664322979 ) ) ;
#6288 = CARTESIAN_POINT ( 'NONE',  ( -13.90420332777824441, 182.5345320759501249, 310.4363584572501509 ) ) ;
#6289 = ORIENTED_EDGE ( 'NONE', *, *, #8066, .F. ) ;
#6290 = ORIENTED_EDGE ( 'NONE', *, *, #3610, .T. ) ;
#6291 = CONICAL_SURFACE ( 'NONE', #8124, 3.309500000000006992, 0.7853981633974710386 ) ;
#6292 = AXIS2_PLACEMENT_3D ( 'NONE', #3102, #12069, #1395 ) ;
#6293 = DIRECTION ( 'NONE',  ( 0.01096700916508646859, -0.5290868411612599242, 0.8484968115555724388 ) ) ;
#6294 = EDGE_CURVE ( 'NONE', #6123, #16406, #4281, .T. ) ;
#6295 = VECTOR ( 'NONE', #20521, 1000.000000000000000 ) ;
#6296 = ORIENTED_EDGE ( 'NONE', *, *, #11840, .F. ) ;
#6297 = CYLINDRICAL_SURFACE ( 'NONE', #2156, 126.0000000000000000 ) ;
#6298 = DIRECTION ( 'NONE',  ( 0.1136178953597579422, -0.9935164314186355483, 0.004009283626633659663 ) ) ;
#6299 = DIRECTION ( 'NONE',  ( 0.007371307436792259166, -0.7031977520565497741, 0.7109561064716214407 ) ) ;
#6300 = ORIENTED_EDGE ( 'NONE', *, *, #12705, .F. ) ;
#6301 = CARTESIAN_POINT ( 'NONE',  ( 11.97603105386089872, 187.6983616241384709, 304.8864109523329375 ) ) ;
#6302 = AXIS2_PLACEMENT_3D ( 'NONE', #12228, #14296, #5536 ) ;
#6303 = CARTESIAN_POINT ( 'NONE',  ( -15.37900450013992604, 178.0904888174965492, 312.5271116413751997 ) ) ;
#6304 = ORIENTED_EDGE ( 'NONE', *, *, #292, .T. ) ;
#6305 = DIRECTION ( 'NONE',  ( 2.025474946048326158E-22, -1.000000000000000000, 1.876735158486679638E-22 ) ) ;
#6306 =( GEOMETRIC_REPRESENTATION_CONTEXT ( 3 ) GLOBAL_UNCERTAINTY_ASSIGNED_CONTEXT ( ( #13220 ) ) GLOBAL_UNIT_ASSIGNED_CONTEXT ( ( #14442, #9114, #10518 ) ) REPRESENTATION_CONTEXT ( 'NONE', 'WORKASPACE' ) );
#6307 = CARTESIAN_POINT ( 'NONE',  ( -38.81316173502003863, 96.91662645125910558, 84.24247758608711933 ) ) ;
#6308 = CARTESIAN_POINT ( 'NONE',  ( -7.374421360215808186, 323.5613325621246190, 320.3790860758305712 ) ) ;
#6309 = ORIENTED_EDGE ( 'NONE', *, *, #15264, .T. ) ;
#6310 = ADVANCED_FACE ( 'NONE', ( #14548 ), #6022, .F. ) ;
#6311 = DIRECTION ( 'NONE',  ( -0.01292394549866737220, -0.005513023399721000799, -0.9999012842304692006 ) ) ;
#6312 = VECTOR ( 'NONE', #20691, 999.9999999999998863 ) ;
#6313 = DIRECTION ( 'NONE',  ( -7.125109674070808144E-05, 0.9999848031710253382, -0.005512562950849314580 ) ) ;
#6314 = VERTEX_POINT ( 'NONE', #14783 ) ;
#6315 = B_SPLINE_CURVE_WITH_KNOTS ( 'NONE', 3,
 ( #22476, #17228, #15638, #8598 ),
 .UNSPECIFIED., .F., .F.,
 ( 4, 4 ),
 ( 0.000000000000000000, 0.001461243987307901107 ),
 .UNSPECIFIED. ) ;
#6316 = UNCERTAINTY_MEASURE_WITH_UNIT (LENGTH_MEASURE( 1.000000000000000082E-05 ), #10965, 'distance_accuracy_value', 'NONE');
#6317 = AXIS2_PLACEMENT_3D ( 'NONE', #4812, #22161, #7004 ) ;
#6318 = B_SPLINE_CURVE_WITH_KNOTS ( 'NONE', 3,
 ( #6350, #9897, #22166, #16918, #8285, #10016 ),
 .UNSPECIFIED., .F., .F.,
 ( 4, 2, 4 ),
 ( 0.009270618776430242583, 0.01189894710419334839, 0.01452727543195645593 ),
 .UNSPECIFIED. ) ;
#6319 = DIRECTION ( 'NONE',  ( 0.009760756503427876415, -0.9999378516499564107, 0.005387065077611007807 ) ) ;
#6320 = CIRCLE ( 'NONE', #20241, 6.000000000000003553 ) ;
#6321 =( GEOMETRIC_REPRESENTATION_CONTEXT ( 3 ) GLOBAL_UNCERTAINTY_ASSIGNED_CONTEXT ( ( #14301 ) ) GLOBAL_UNIT_ASSIGNED_CONTEXT ( ( #12616, #7199, #13988 ) ) REPRESENTATION_CONTEXT ( 'NONE', 'WORKASPACE' ) );
#6322 = DIRECTION ( 'NONE',  ( 0.01035335185279115042, 0.005513005182354825326, 0.9999312050732648283 ) ) ;
#6323 = EDGE_CURVE ( 'NONE', #21650, #5831, #4056, .T. ) ;
#6324 = SHAPE_DEFINITION_REPRESENTATION ( #1892, #9590 ) ;
#6325 = VERTEX_POINT ( 'NONE', #18310 ) ;
#6326 = DIRECTION ( 'NONE',  ( -0.000000000000000000, -1.000000000000000000, -0.000000000000000000 ) ) ;
#6327 = CARTESIAN_POINT ( 'NONE',  ( -52.81114432656352875, 109.8083481694280721, -43.48992680558292534 ) ) ;
#6328 = ORIENTED_EDGE ( 'NONE', *, *, #7731, .F. ) ;
#6329 = DIRECTION ( 'NONE',  ( 0.000000000000000000, 0.000000000000000000, -1.000000000000000000 ) ) ;
#6330 = AXIS2_PLACEMENT_3D ( 'NONE', #6010, #20007, #4271 ) ;
#6331 = CARTESIAN_POINT ( 'NONE',  ( -33.82085273160089400, 93.50464841319747222, 82.93470554904384073 ) ) ;
#6332 = PLANE ( 'NONE',  #17467 ) ;
#6333 = DIRECTION ( 'NONE',  ( 0.9999164797902017066, 0.000000000000000000, -0.01292414190464157529 ) ) ;
#6334 = DIRECTION ( 'NONE',  ( 0.01292414190464131508, 0.000000000000000000, 0.9999164797902017066 ) ) ;
#6335 = ORIENTED_EDGE ( 'NONE', *, *, #3564, .T. ) ;
#6336 = PLANE ( 'NONE',  #11363 ) ;
#6337 = LINE ( 'NONE', #16906, #16840 ) ;
#6338 = ORIENTED_EDGE ( 'NONE', *, *, #13322, .T. ) ;
#6339 = FACE_OUTER_BOUND ( 'NONE', #2451, .T. ) ;
#6340 = CARTESIAN_POINT ( 'NONE',  ( -65.67450334697799974, 189.7102623349352086, -51.76499945731497121 ) ) ;
#6341 = DIRECTION ( 'NONE',  ( 0.01292414190464131335, 1.902755938799530239E-22, 0.9999164797902015955 ) ) ;
#6342 = DIRECTION ( 'NONE',  ( 0.9999164797902017066, 0.000000000000000000, -0.01292414190463751951 ) ) ;
#6343 = AXIS2_PLACEMENT_3D ( 'NONE', #10609, #12884, #9415 ) ;
#6344 = AXIS2_PLACEMENT_3D ( 'NONE', #5303, #16136, #15912 ) ;
#6345 = ORIENTED_EDGE ( 'NONE', *, *, #8487, .F. ) ;
#6346 = ADVANCED_FACE ( 'NONE', ( #14899 ), #19798, .T. ) ;
#6347 = CARTESIAN_POINT ( 'NONE',  ( -49.64894119642055870, 126.1473026246197406, 27.48387445644694083 ) ) ;
#6348 = EDGE_CURVE ( 'NONE', #7061, #4119, #11399, .T. ) ;
#6349 = ORIENTED_EDGE ( 'NONE', *, *, #13250, .F. ) ;
#6350 = CARTESIAN_POINT ( 'NONE',  ( 5.149300590115022835, 81.19615242270661781, -98.24794683011701579 ) ) ;
#6351 = CYLINDRICAL_SURFACE ( 'NONE', #816, 4.000000000000002665 ) ;
#6352 = ORIENTED_EDGE ( 'NONE', *, *, #4149, .T. ) ;
#6353 = FACE_OUTER_BOUND ( 'NONE', #2813, .T. ) ;
#6354 = CARTESIAN_POINT ( 'NONE',  ( -90.09729892282578589, 88.47696219913342475, 52.76108841404412431 ) ) ;
#6356 = FACE_OUTER_BOUND ( 'NONE', #4392, .T. ) ;
#6355 = VECTOR ( 'NONE', #6651, 999.9999999999998863 ) ;
#6357 = VERTEX_POINT ( 'NONE', #18215 ) ;
#6358 = AXIS2_PLACEMENT_3D ( 'NONE', #12418, #3556, #5155 ) ;
#6359 = DIRECTION ( 'NONE',  ( -1.000000000000000000, 0.000000000000000000, -1.362186893977296347E-14 ) ) ;
#6360 = VERTEX_POINT ( 'NONE', #21840 ) ;
#6361 = DIRECTION ( 'NONE',  ( 0.01292394549866727679, 0.005513023399720742325, 0.9999012842304692006 ) ) ;
#6362 = LINE ( 'NONE', #4717, #15569 ) ;
#6363 = CARTESIAN_POINT ( 'NONE',  ( 161.9999999999992610, 20.00000000000000000, 53.76161406891478123 ) ) ;
#6364 = VERTEX_POINT ( 'NONE', #6132 ) ;
#6365 = CARTESIAN_POINT ( 'NONE',  ( -63.92582232734818604, 91.13550884953522768, 66.60804284595937474 ) ) ;
#6366 = DIRECTION ( 'NONE',  ( -0.01292394549866736873, -0.005513023399717647578, -0.9999012842304690896 ) ) ;
#6367 = AXIS2_PLACEMENT_3D ( 'NONE', #13744, #13515, #2825 ) ;
#6368 = CARTESIAN_POINT ( 'NONE',  ( 19.84368754553128866, 183.6791006555748424, 315.4184450387429592 ) ) ;
#6369 = B_SPLINE_CURVE_WITH_KNOTS ( 'NONE', 3,
 ( #16301, #646, #7634, #6041 ),
 .UNSPECIFIED., .F., .F.,
 ( 4, 4 ),
 ( 0.000000000000000000, 0.001461243987308225717 ),
 .UNSPECIFIED. ) ;
#6370 = CARTESIAN_POINT ( 'NONE',  ( -90.00466877033377955, 70.05991977044968166, 63.23890890537643372 ) ) ;
#6371 = B_SPLINE_CURVE_WITH_KNOTS ( 'NONE', 3,
 ( #2522, #3897, #10915, #9525, #810, #6080, #7809, #21790, #4337, #9866, #11490, #22238, #14950, #18594, #21896, #16888, #13337, #22011 ),
 .UNSPECIFIED., .F., .F.,
 ( 4, 2, 2, 2, 2, 2, 2, 2, 4 ),
 ( -3.889482229076588469E-05, 0.0005389813425374914355, 0.001116857507365748769, 0.001694733672194006103, 0.002272609837022263653, 0.002850486001850521204, 0.003428362166678778321, 0.004006238331507035004, 0.004584114496335292555 ),
 .UNSPECIFIED. ) ;
#6372 = CARTESIAN_POINT ( 'NONE',  ( -1.632550740186645921, 142.7036636415817838, 274.8672572718562037 ) ) ;
#6373 = ORIENTED_EDGE ( 'NONE', *, *, #14305, .T. ) ;
#6374 = CARTESIAN_POINT ( 'NONE',  ( 0.000000000000000000, 0.000000000000000000, 0.000000000000000000 ) ) ;
#6375 = VECTOR ( 'NONE', #14801, 1000.000000000000000 ) ;
#6376 = AXIS2_PLACEMENT_3D ( 'NONE', #5429, #1672, #49 ) ;
#6377 = DIRECTION ( 'NONE',  ( 0.009760756503428009989, -0.9999378516499564107, 0.005387065077611111891 ) ) ;
#6378 = CARTESIAN_POINT ( 'NONE',  ( -64.02441888546434257, 100.0345687961148826, 75.89892270379247918 ) ) ;
#6379 = ORIENTED_EDGE ( 'NONE', *, *, #12796, .T. ) ;
#6380 = CARTESIAN_POINT ( 'NONE',  ( -10.44786468173362337, 186.3147661259626204, 278.0874267879351009 ) ) ;
#6381 = ORIENTED_EDGE ( 'NONE', *, *, #13766, .F. ) ;
#6382 = ORIENTED_EDGE ( 'NONE', *, *, #20850, .T. ) ;
#6383 = CARTESIAN_POINT ( 'NONE',  ( 0.6170534444071897884, 95.45144721132757581, 47.74026101898994767 ) ) ;
#6384 = AXIS2_PLACEMENT_3D ( 'NONE', #18329, #6156, #8940 ) ;
#6385 = VERTEX_POINT ( 'NONE', #16494 ) ;
#6386 = CARTESIAN_POINT ( 'NONE',  ( -64.28883878761490678, 83.29019440189556178, 55.44125366118054643 ) ) ;
#6387 = FACE_OUTER_BOUND ( 'NONE', #3453, .T. ) ;
#6388 = AXIS2_PLACEMENT_3D ( 'NONE', #13952, #12465, #8883 ) ;
#6389 = AXIS2_PLACEMENT_3D ( 'NONE', #13669, #10642, #15723 ) ;
#6390 = CARTESIAN_POINT ( 'NONE',  ( -8.232661088767551760, 109.6915715130226232, 125.7263821215522341 ) ) ;
#6391 = DIRECTION ( 'NONE',  ( -0.000000000000000000, -1.000000000000000000, -0.000000000000000000 ) ) ;
#6392 = DIRECTION ( 'NONE',  ( 5.440186201345738641E-18, 1.000000000000000000, 1.334940939666364181E-17 ) ) ;
#6393 = DIRECTION ( 'NONE',  ( -0.01292394549866745720, -0.005513023399720816918, -0.9999012842304692006 ) ) ;
#6394 = CARTESIAN_POINT ( 'NONE',  ( 41.33663990117435816, 95.22970684149694875, 83.53052428595084677 ) ) ;
#6395 = FACE_OUTER_BOUND ( 'NONE', #5424, .T. ) ;
#6396 = CARTESIAN_POINT ( 'NONE',  ( -68.69096839185023384, 69.99999999999998579, 87.89511284132827029 ) ) ;
#6397 = ADVANCED_FACE ( 'NONE', ( #20365 ), #6804, .T. ) ;
#6398 = CARTESIAN_POINT ( 'NONE',  ( 90.61229378181252514, 77.84360403296375353, -32.30868923918635005 ) ) ;
#6399 = CARTESIAN_POINT ( 'NONE',  ( -55.40268456415264353, 20.00000000000000000, -113.1659955246495883 ) ) ;
#6400 = AXIS2_PLACEMENT_3D ( 'NONE', #22037, #10007, #4810 ) ;
#6401 = EDGE_CURVE ( 'NONE', #11384, #5047, #1087, .T. ) ;
#6402 = EDGE_LOOP ( 'NONE', ( #8469, #19215, #12209, #359 ) ) ;
#6403 = CARTESIAN_POINT ( 'NONE',  ( -43.33363090647537774, 163.6553657754814992, 273.2207310035200294 ) ) ;
#6404 = CARTESIAN_POINT ( 'NONE',  ( -14.03868214994468211, 180.1681535970077164, 308.8297336107179376 ) ) ;
#6405 = ORIENTED_EDGE ( 'NONE', *, *, #4986, .F. ) ;
#6406 = CIRCLE ( 'NONE', #533, 75.00000000000002842 ) ;
#6407 = EDGE_LOOP ( 'NONE', ( #5098, #19621, #11532, #1873 ) ) ;
#6408 = B_SPLINE_CURVE_WITH_KNOTS ( 'NONE', 3,
 ( #14265, #16348, #2525, #587, #7580, #17940, #21467, #18169, #9409, #12874, #5728, #2420, #12761, #13005, #4236, #470 ),
 .UNSPECIFIED., .F., .F.,
 ( 4, 2, 2, 2, 2, 2, 2, 4 ),
 ( -2.211772431870429045E-17, 0.0003967982407998327829, 0.0007935964815996876835, 0.001190394722399542530, 0.001587192963199397485, 0.001983991203999252440, 0.002380789444799107177, 0.003174385926398843108 ),
 .UNSPECIFIED. ) ;
#6409 = CARTESIAN_POINT ( 'NONE',  ( -66.45999312048353147, 70.00000000000000000, 87.65380681892987980 ) ) ;
#6410 = EDGE_CURVE ( 'NONE', #10365, #3828, #15238, .T. ) ;
#6411 = VECTOR ( 'NONE', #6634, 1000.000000000000227 ) ;
#6412 = ORIENTED_EDGE ( 'NONE', *, *, #4860, .F. ) ;
#6413 = CARTESIAN_POINT ( 'NONE',  ( -1.163172771417704698, 45.00000000000000000, -89.99248318111816047 ) ) ;
#6414 = DIRECTION ( 'NONE',  ( -0.01292394549866739996, -0.005513023399721131770, -0.9999012842304692006 ) ) ;
#6415 = ADVANCED_FACE ( 'NONE', ( #3022 ), #12070, .F. ) ;
#6416 = FACE_OUTER_BOUND ( 'NONE', #8783, .T. ) ;
#6417 = ORIENTED_EDGE ( 'NONE', *, *, #2258, .F. ) ;
#6418 = ORIENTED_EDGE ( 'NONE', *, *, #7525, .F. ) ;
#6419 = AXIS2_PLACEMENT_3D ( 'NONE', #15516, #11946, #6645 ) ;
#6420 = CARTESIAN_POINT ( 'NONE',  ( -93.23587179807654479, 69.99999999999998579, -30.79757858250321689 ) ) ;
#6421 = CARTESIAN_POINT ( 'NONE',  ( -57.55251350461809778, 118.9484885890504557, 172.9440730829682877 ) ) ;
#6422 = LINE ( 'NONE', #17106, #21771 ) ;
#6423 = FACE_OUTER_BOUND ( 'NONE', #1868, .T. ) ;
#6424 = ORIENTED_EDGE ( 'NONE', *, *, #17203, .F. ) ;
#6425 = EDGE_CURVE ( 'NONE', #19042, #15351, #4410, .T. ) ;
#6426 = DIRECTION ( 'NONE',  ( -0.9999164797902015955, -4.476705744456278510E-15, 0.01292414190463697134 ) ) ;
#6427 = EDGE_CURVE ( 'NONE', #3659, #22165, #9181, .T. ) ;
#6428 = ADVANCED_FACE ( 'NONE', ( #4959 ), #15452, .F. ) ;
#6429 = DIRECTION ( 'NONE',  ( -2.025474946048326158E-22, 1.000000000000000000, -1.876735158486678933E-22 ) ) ;
#6430 = CARTESIAN_POINT ( 'NONE',  ( 11.42559457476033025, 143.4049563503333786, 275.1388332802161472 ) ) ;
#6431 = ADVANCED_FACE ( 'NONE', ( #22617 ), #15787, .F. ) ;
#6432 = STYLED_ITEM ( 'NONE', ( #19993 ), #9632 ) ;
#6433 = EDGE_CURVE ( 'NONE', #1407, #2837, #5526, .T. ) ;
#6434 = CARTESIAN_POINT ( 'NONE',  ( -23.46300067765492514, 324.6023353951521813, 307.6447243945494279 ) ) ;
#6435 = EDGE_LOOP ( 'NONE', ( #22362, #1224, #14750, #6163 ) ) ;
#6436 = CARTESIAN_POINT ( 'NONE',  ( 7.145902869757795983, 69.99999999999998579, -93.45069977196735067 ) ) ;
#6437 = DIRECTION ( 'NONE',  ( -0.000000000000000000, 1.000000000000000000, -0.000000000000000000 ) ) ;
#6438 = APPLICATION_PROTOCOL_DEFINITION ( 'draft international standard', 'automotive_design', 1998, #3831 ) ;
#6439 = ORIENTED_EDGE ( 'NONE', *, *, #6278, .T. ) ;
#6440 = CARTESIAN_POINT ( 'NONE',  ( 91.12451015595509318, 77.41163679146359300, -31.64200013680036605 ) ) ;
#6441 = ADVANCED_FACE ( 'NONE', ( #12224 ), #3818, .T. ) ;
#6442 = VERTEX_POINT ( 'NONE', #7036 ) ;
#6443 = FACE_OUTER_BOUND ( 'NONE', #14951, .T. ) ;
#6444 = LINE ( 'NONE', #4352, #9998 ) ;
#6445 = AXIS2_PLACEMENT_3D ( 'NONE', #1511, #7125, #19405 ) ;
#6446 = CARTESIAN_POINT ( 'NONE',  ( 4.917494328089510702, 81.92338897118681018, -83.12797620812510502 ) ) ;
#6447 = DIRECTION ( 'NONE',  ( -0.9999164797902015955, -6.965998958219364448E-18, 0.01292414190464157182 ) ) ;
#6448 = LINE ( 'NONE', #11506, #158 ) ;
#6449 = ORIENTED_EDGE ( 'NONE', *, *, #9115, .T. ) ;
#6450 = DIRECTION ( 'NONE',  ( -0.7944560844389302323, 1.242937374672305755E-17, -0.6073216033519337476 ) ) ;
#6451 = DIRECTION ( 'NONE',  ( -7.125109674161246868E-05, 0.9999848031710252272, -0.005512562950850154186 ) ) ;
#6452 = ORIENTED_EDGE ( 'NONE', *, *, #4283, .T. ) ;
#6453 = DIRECTION ( 'NONE',  ( 0.7161863329816247070, 0.003898296230784560612, 0.6978982302147144212 ) ) ;
#6454 = CARTESIAN_POINT ( 'NONE',  ( -56.08328763590613164, 143.6018742220275044, 109.9799478008652613 ) ) ;
#6455 = DIRECTION ( 'NONE',  ( -0.01292394549866738608, -0.005513023399720699824, -0.9999012842304692006 ) ) ;
#6456 = LINE ( 'NONE', #13800, #19501 ) ;
#6457 = ADVANCED_FACE ( 'NONE', ( #15910 ), #5405, .F. ) ;
#6458 = DIRECTION ( 'NONE',  ( 0.01292414190464179213, 0.000000000000000000, 0.9999164797902017066 ) ) ;
#6459 = ORIENTED_EDGE ( 'NONE', *, *, #110, .T. ) ;
#6460 = LINE ( 'NONE', #15319, #2861 ) ;
#6461 = PLANE ( 'NONE',  #11806 ) ;
#6462 = ORIENTED_EDGE ( 'NONE', *, *, #11910, .F. ) ;
#6463 = VECTOR ( 'NONE', #15305, 1000.000000000000227 ) ;
#6464 = DIRECTION ( 'NONE',  ( 0.01292394549866733404, 0.005513023399720420534, 0.9999012842304693116 ) ) ;
#6465 = CARTESIAN_POINT ( 'NONE',  ( -90.00978037925260367, 88.71181518729869708, 52.51177033982978770 ) ) ;
#6466 = DIRECTION ( 'NONE',  ( -0.9999164797902015955, -8.772500386246549315E-18, 0.01292414190464155101 ) ) ;
#6467 = ORIENTED_EDGE ( 'NONE', *, *, #21009, .F. ) ;
#6468 = EDGE_CURVE ( 'NONE', #20544, #12076, #12039, .T. ) ;
#6469 = CARTESIAN_POINT ( 'NONE',  ( -75.24529543015454180, 95.02827877570439341, 80.23810401866792574 ) ) ;
#6470 = PLANE ( 'NONE',  #7042 ) ;
#6471 = DIRECTION ( 'NONE',  ( -0.9934404589540162256, -0.1135548637187056842, 0.01346653032743081423 ) ) ;
#6472 = CARTESIAN_POINT ( 'NONE',  ( -35.77069358118214382, 165.3260487394316840, 277.1141618424657054 ) ) ;
#6473 = CARTESIAN_POINT ( 'NONE',  ( -88.17696233076783585, 88.99987371843837991, 51.57339716971453925 ) ) ;
#6474 = DIRECTION ( 'NONE',  ( 0.000000000000000000, 0.000000000000000000, 1.000000000000000000 ) ) ;
#6475 = CARTESIAN_POINT ( 'NONE',  ( -56.11438623100815448, 126.5883500096207683, 107.5739081604535414 ) ) ;
#6476 = ORIENTED_EDGE ( 'NONE', *, *, #742, .T. ) ;
#6477 = EDGE_LOOP ( 'NONE', ( #21042, #18427, #4181, #13987, #3507, #12855, #15167 ) ) ;
#6478 = DIRECTION ( 'NONE',  ( 0.000000000000000000, -1.000000000000000000, 0.000000000000000000 ) ) ;
#6479 = CARTESIAN_POINT ( 'NONE',  ( 67.23655452815148692, 145.1029152106949027, 17.86880078497820179 ) ) ;
#6480 = CARTESIAN_POINT ( 'NONE',  ( 1.117803423002110774, 45.00000000000000000, 109.6947150755565161 ) ) ;
#6481 = DIRECTION ( 'NONE',  ( -7.125109674160258889E-05, 0.9999848031710252272, -0.005512562950849897447 ) ) ;
#6482 = CARTESIAN_POINT ( 'NONE',  ( -8.417507809094315618, 145.3803201924227153, 276.8538022553906899 ) ) ;
#6483 = ORIENTED_EDGE ( 'NONE', *, *, #9973, .T. ) ;
#6484 =( NAMED_UNIT ( * ) PLANE_ANGLE_UNIT ( ) SI_UNIT ( $, .RADIAN. ) );
#6485 = DIRECTION ( 'NONE',  ( -7.125109674243555432E-05, 0.9999848031710253382, -0.005512562950850175003 ) ) ;
#6486 = CARTESIAN_POINT ( 'NONE',  ( -11.79663605375380975, 185.7023549694303313, 320.6758801748541714 ) ) ;
#6487 = VERTEX_POINT ( 'NONE', #19320 ) ;
#6488 = CARTESIAN_POINT ( 'NONE',  ( -9.289650516680991288, 187.1478790530904348, 276.7252570793428390 ) ) ;
#6489 = ORIENTED_EDGE ( 'NONE', *, *, #1241, .F. ) ;
#6490 = LINE ( 'NONE', #13504, #11924 ) ;
#6492 = ORIENTED_EDGE ( 'NONE', *, *, #9407, .T. ) ;
#6491 = EDGE_LOOP ( 'NONE', ( #18356, #14484, #10502 ) ) ;
#6493 = EDGE_CURVE ( 'NONE', #4942, #21601, #4780, .T. ) ;
#6494 = CARTESIAN_POINT ( 'NONE',  ( -49.57489512272184129, 107.2650309926512193, 71.07430715179511083 ) ) ;
#6495 = DIRECTION ( 'NONE',  ( 7.125109674403838460E-05, -0.9999848031710254492, 0.005512562950847868688 ) ) ;
#6496 = EDGE_CURVE ( 'NONE', #7803, #7424, #6635, .T. ) ;
#6497 = CARTESIAN_POINT ( 'NONE',  ( -109.9283388797385612, 75.00188554563106891, 6.129144436280878239 ) ) ;
#6498 = CARTESIAN_POINT ( 'NONE',  ( -157.5176307659779411, 18.00000000000000355, -60.94675664190618392 ) ) ;
#6499 =( BOUNDED_SURFACE ( )  B_SPLINE_SURFACE ( 3, 2, ( 
 ( #21435, #19813, #4201 ),
 ( #16194, #4082, #11116 ),
 ( #7308, #2037, #432 ),
 ( #5697, #15965, #9140 ),
 ( #7549, #7430, #12728 ),
 ( #7200, #19595, #9023 ),
 ( #19483, #9262, #19696 ),
 ( #12965, #3963, #12617 ),
 ( #314, #14348, #14577 ),
 ( #10987, #3867, #18016 ),
 ( #11229, #10880, #21641 ),
 ( #10770, #18136, #21317 ),
 ( #204, #2260, #17906 ),
 ( #550, #21531, #2387 ),
 ( #14231, #5801, #3757 ),
 ( #12835, #9379, #17800 ),
 ( #16413, #659, #5927 ),
 ( #14690, #19932, #21206 ) ),
 .UNSPECIFIED., .F., .F., .T. ) 
 B_SPLINE_SURFACE_WITH_KNOTS ( ( 4, 2, 2, 2, 2, 2, 2, 2, 4 ),
 ( 3, 3 ),
 ( 0.002597246120634467796, 0.003399884678228190776, 0.004202523235821913755, 0.005005161793415637168, 0.005807800351009360582, 0.006610438908603083995, 0.007413077466196807408, 0.008215716023790529954, 0.009018354581384254234 ),
 ( 0.000000000000000000, 1.000000000000000000 ),
 .UNSPECIFIED. ) 
 GEOMETRIC_REPRESENTATION_ITEM ( )  RATIONAL_B_SPLINE_SURFACE ( (
 ( 1.000000000000000000, 0.5963808372950819559, 1.000000000000000000),
 ( 1.000000000000000000, 0.5963839598476180504, 1.000000000000000000),
 ( 1.000000000000000000, 0.5970886094880794026, 1.000000000000000000),
 ( 1.000000000000000000, 0.5998681984913176723, 1.000000000000000000),
 ( 1.000000000000000000, 0.6019790828716353737, 1.000000000000000000),
 ( 1.000000000000000000, 0.6074656362385493225, 1.000000000000000000),
 ( 1.000000000000000000, 0.6108290540004431834, 1.000000000000000000),
 ( 1.000000000000000000, 0.6188252630046991998, 1.000000000000000000),
 ( 1.000000000000000000, 0.6234423941985007822, 1.000000000000000000),
 ( 1.000000000000000000, 0.6335838931037276467, 1.000000000000000000),
 ( 1.000000000000000000, 0.6391861101551582491, 1.000000000000000000),
 ( 1.000000000000000000, 0.6512661799281685981, 1.000000000000000000),
 ( 1.000000000000000000, 0.6576333021886564545, 1.000000000000000000),
 ( 1.000000000000000000, 0.6710088154586895115, 1.000000000000000000),
 ( 1.000000000000000000, 0.6780884601156411673, 1.000000000000000000),
 ( 1.000000000000000000, 0.6924279500034853374, 1.000000000000000000),
 ( 1.000000000000000000, 0.6997125326201852902, 1.000000000000000000),
 ( 1.000000000000000000, 0.7071067811865473507, 1.000000000000000000) ) ) 
 REPRESENTATION_ITEM ( '' )  SURFACE ( )  );
#6500 = CARTESIAN_POINT ( 'NONE',  ( 16.79060435579898325, 186.8892895049134779, 277.5964890151019517 ) ) ;
#6501 = CARTESIAN_POINT ( 'NONE',  ( 42.82096601309913808, 94.49577377718297555, 82.85231139482363005 ) ) ;
#6502 = DIRECTION ( 'NONE',  ( -0.9999164797902017066, -2.045753974208586179E-15, 0.01292414190464156835 ) ) ;
#6503 = CARTESIAN_POINT ( 'NONE',  ( -51.34037389809783036, 189.5966443421384611, -72.56069641891028255 ) ) ;
#6504 = CARTESIAN_POINT ( 'NONE',  ( 90.73345939407627725, 80.10652859373304580, -31.90946778207672097 ) ) ;
#6505 = CARTESIAN_POINT ( 'NONE',  ( -146.5000000000000000, 20.00000000000000000, 2.081668171172168513E-14 ) ) ;
#6506 = ORIENTED_EDGE ( 'NONE', *, *, #7582, .T. ) ;
#6507 = ORIENTED_EDGE ( 'NONE', *, *, #10083, .T. ) ;
#6508 = DIRECTION ( 'NONE',  ( 0.01292414190464174703, 0.000000000000000000, 0.9999164797902015955 ) ) ;
#6509 = LINE ( 'NONE', #13524, #4434 ) ;
#6510 = VERTEX_POINT ( 'NONE', #1755 ) ;
#6511 = DIRECTION ( 'NONE',  ( -0.01292414190464131335, 0.000000000000000000, -0.9999164797902017066 ) ) ;
#6512 = ORIENTED_EDGE ( 'NONE', *, *, #19767, .F. ) ;
#6513 = FACE_OUTER_BOUND ( 'NONE', #15526, .T. ) ;
#6514 = EDGE_CURVE ( 'NONE', #12381, #4519, #5301, .T. ) ;
#6515 = ORIENTED_EDGE ( 'NONE', *, *, #15113, .F. ) ;
#6516 = DIRECTION ( 'NONE',  ( 2.025474946048326158E-22, -1.000000000000000000, 1.876735158486679638E-22 ) ) ;
#6517 = CARTESIAN_POINT ( 'NONE',  ( 11.46456758449441971, 143.4062123375417457, 275.1480316732433948 ) ) ;
#6518 = CARTESIAN_POINT ( 'NONE',  ( 14.61723280919641255, 187.0110612265052339, 320.7690430450153372 ) ) ;
#6519 = VERTEX_POINT ( 'NONE', #1990 ) ;
#6521 = FACE_OUTER_BOUND ( 'NONE', #21886, .T. ) ;
#6520 = B_SPLINE_CURVE_WITH_KNOTS ( 'NONE', 3,
 ( #11255, #5835, #5722, #14834, #7911, #2636, #12755, #9521, #16552, #5959, #18162, #806, #3894, #21891, #9402, #21785, #14607, #2169, #9168, #6076, #14947, #16439, #19626, #7575, #20072, #10910, #462, #689 ),
 .UNSPECIFIED., .F., .F.,
 ( 4, 2, 2, 2, 2, 2, 2, 2, 2, 2, 2, 2, 2, 4 ),
 ( 0.006298532399469917130, 0.01550158377817707420, 0.02010310946753066097, 0.02240387231220746303, 0.02470463515688426162, 0.03390768653559145251, 0.03850921222494505664, 0.04080997506962185523, 0.04311073791429865382, 0.05231378929300583430, 0.06151684067171302867, 0.06611836636106661891, 0.07071989205042020221, 0.07992294342912738270 ),
 .UNSPECIFIED. ) ;
#6522 = CARTESIAN_POINT ( 'NONE',  ( 110.0212991616529052, 74.99906874937914836, 0.8747890471060546513 ) ) ;
#6523 = DIRECTION ( 'NONE',  ( 0.01292394549866733230, 0.005513023399720419666, 0.9999012842304692006 ) ) ;
#6524 = ORIENTED_EDGE ( 'NONE', *, *, #10212, .T. ) ;
#6525 = FACE_OUTER_BOUND ( 'NONE', #12109, .T. ) ;
#6526 = EDGE_CURVE ( 'NONE', #13001, #18202, #3584, .T. ) ;
#6527 = EDGE_LOOP ( 'NONE', ( #2608, #17702 ) ) ;
#6528 = DIRECTION ( 'NONE',  ( 0.9999164797902017066, 2.001050586498416282E-22, -0.01292414190464117631 ) ) ;
#6529 = CARTESIAN_POINT ( 'NONE',  ( -12.58664483627160990, 184.6272112293441694, 320.1917372557447834 ) ) ;
#6530 = AXIS2_PLACEMENT_3D ( 'NONE', #15952, #14103, #10631 ) ;
#6531 = DIRECTION ( 'NONE',  ( -0.01292414190464022741, 0.000000000000000000, -0.9999164797902017066 ) ) ;
#6532 = DIRECTION ( 'NONE',  ( 0.01035335185279134471, 0.005513005182356394383, 0.9999312050732649393 ) ) ;
#6533 = CARTESIAN_POINT ( 'NONE',  ( 51.39870305934242367, 113.4706157781613598, -46.85725176872078634 ) ) ;
#6534 = APPLICATION_PROTOCOL_DEFINITION ( 'draft international standard', 'automotive_design', 1998, #16460 ) ;
#6535 = CIRCLE ( 'NONE', #3214, 3.399999999999986144 ) ;
#6536 = EDGE_CURVE ( 'NONE', #16597, #5442, #18025, .T. ) ;
#6537 = EDGE_LOOP ( 'NONE', ( #21168, #13651, #7264, #7528 ) ) ;
#6538 = ADVANCED_FACE ( 'NONE', ( #16026 ), #154, .T. ) ;
#6539 = CARTESIAN_POINT ( 'NONE',  ( -10.85624112972181621, 113.6998737626107641, 127.2553023597115498 ) ) ;
#6540 = DIRECTION ( 'NONE',  ( -0.01292394549866736873, -0.005513023399721228915, -0.9999012842304690896 ) ) ;
#6541 = DIRECTION ( 'NONE',  ( 0.9232306267972768543, 0.000000000000000000, -0.3842462878721241704 ) ) ;
#6542 = DIRECTION ( 'NONE',  ( -0.01292414190464022741, 0.000000000000000000, -0.9999164797902017066 ) ) ;
#6543 = DIRECTION ( 'NONE',  ( 0.000000000000000000, 1.000000000000000000, -0.000000000000000000 ) ) ;
#6544 = DIRECTION ( 'NONE',  ( -0.9770372205688160339, 0.2127605332646582970, 0.01145535281434409587 ) ) ;
#6545 = AXIS2_PLACEMENT_3D ( 'NONE', #10732, #10849, #14198 ) ;
#6546 = ORIENTED_EDGE ( 'NONE', *, *, #5354, .T. ) ;
#6547 = CARTESIAN_POINT ( 'NONE',  ( 51.15696624816380478, 110.0038319760128189, -44.83481546877135315 ) ) ;
#6548 = VERTEX_POINT ( 'NONE', #1867 ) ;
#6549 = CARTESIAN_POINT ( 'NONE',  ( -40.94831321612058161, 169.5761513248267818, 277.1576504944517296 ) ) ;
#6550 = DIRECTION ( 'NONE',  ( 7.125109674160258889E-05, -0.9999848031710253382, 0.005512562950849898315 ) ) ;
#6551 = CARTESIAN_POINT ( 'NONE',  ( 105.8297815006158515, 70.09865364193531434, 30.00121230636247560 ) ) ;
#6552 = DIRECTION ( 'NONE',  ( -0.01292394549866742771, -0.005513023399720295634, -0.9999012842304693116 ) ) ;
#6553 = EDGE_CURVE ( 'NONE', #18095, #18970, #14180, .T. ) ;
#6554 = EDGE_LOOP ( 'NONE', ( #19637, #21634, #4407, #16604 ) ) ;
#6555 = DIRECTION ( 'NONE',  ( -0.01292414190464131335, -1.902755938799530239E-22, -0.9999164797902015955 ) ) ;
#6556 = DIRECTION ( 'NONE',  ( 0.9999164797902017066, 2.001050586450178931E-22, -0.01292414190464131508 ) ) ;
#6557 = CARTESIAN_POINT ( 'NONE',  ( 17.14183078491316436, 175.4877217292663545, 88.23789649046089778 ) ) ;
#6558 = AXIS2_PLACEMENT_3D ( 'NONE', #16836, #20128, #16499 ) ;
#6559 = VERTEX_POINT ( 'NONE', #18080 ) ;
#6560 = CARTESIAN_POINT ( 'NONE',  ( -41.41899454747532161, 166.0889136240114681, 277.1829612759436827 ) ) ;
#6561 = EDGE_CURVE ( 'NONE', #1692, #4043, #2198, .T. ) ;
#6562 = CYLINDRICAL_SURFACE ( 'NONE', #2265, 7.499999999999992006 ) ;
#6563 = VECTOR ( 'NONE', #10020, 1000.000000000000114 ) ;
#6564 = ORIENTED_EDGE ( 'NONE', *, *, #16572, .F. ) ;
#6565 = CARTESIAN_POINT ( 'NONE',  ( 20.99042507241804145, 140.4227465520236819, 76.49807275461785139 ) ) ;
#6566 = CARTESIAN_POINT ( 'NONE',  ( -90.12508629359015799, 87.39786947457938027, 51.15624717128011412 ) ) ;
#6567 = EDGE_LOOP ( 'NONE', ( #876, #21816, #10845, #21999 ) ) ;
#6568 = EDGE_CURVE ( 'NONE', #4488, #440, #14755, .T. ) ;
#6569 = DIRECTION ( 'NONE',  ( -2.025474946048326393E-22, 1.000000000000000000, -1.876735158486679873E-22 ) ) ;
#6570 = DIRECTION ( 'NONE',  ( 0.01292394549866733230, 0.005513023399720419666, 0.9999012842304692006 ) ) ;
#6571 = DIRECTION ( 'NONE',  ( 0.000000000000000000, 0.000000000000000000, 1.000000000000000000 ) ) ;
#6572 = LINE ( 'NONE', #17260, #16869 ) ;
#6573 = CIRCLE ( 'NONE', #9506, 126.0000000000000000 ) ;
#6574 = CARTESIAN_POINT ( 'NONE',  ( -89.24856274066354445, 79.52628152566919084, 30.13108863562646533 ) ) ;
#6575 = CARTESIAN_POINT ( 'NONE',  ( -9.065023647928146744, 109.7167603697149474, 130.3064260814875013 ) ) ;
#6576 = VERTEX_POINT ( 'NONE', #2961 ) ;
#6577 = TOROIDAL_SURFACE ( 'NONE', #16152, 4.000000000000000000, 2.000000000000000000 ) ;
#6578 = FACE_OUTER_BOUND ( 'NONE', #4728, .T. ) ;
#6579 = LINE ( 'NONE', #9809, #14083 ) ;
#6580 = CARTESIAN_POINT ( 'NONE',  ( 16.70266120485480243, 187.6440219821165840, 319.6249571544858554 ) ) ;
#6581 = DIRECTION ( 'NONE',  ( -2.025474946048326158E-22, 1.000000000000000000, -1.876735158486678933E-22 ) ) ;
#6582 = CARTESIAN_POINT ( 'NONE',  ( -3.813579275066386387, 143.2905249558850755, 275.5763592733787277 ) ) ;
#6583 = DIRECTION ( 'NONE',  ( 0.01292394549866747802, 0.005513023399721269681, 0.9999012842304692006 ) ) ;
#6584 = B_SPLINE_CURVE_WITH_KNOTS ( 'NONE', 3,
 ( #9051, #17836, #16105, #21234, #14260, #14386, #2072, #7465, #12656, #12531, #7577, #14501, #19628, #3896, #10913, #17936 ),
 .UNSPECIFIED., .F., .F.,
 ( 4, 2, 2, 2, 2, 2, 2, 4 ),
 ( -3.123367963890199151E-05, 0.001725203944011580084, 0.003481641567662062051, 0.006994516814963025984, 0.008750954438613504915, 0.01050739206226398471, 0.01226382968591446451, 0.01402026730956494605 ),
 .UNSPECIFIED. ) ;
#6585 = ADVANCED_FACE ( 'NONE', ( #6525 ), #10939, .F. ) ;
#6586 = DIRECTION ( 'NONE',  ( -0.01292394549866738608, -0.005513023399721785761, -0.9999012842304693116 ) ) ;
#6587 = ORIENTED_EDGE ( 'NONE', *, *, #4476, .T. ) ;
#6588 = CARTESIAN_POINT ( 'NONE',  ( -7.645763215668887725, 188.5431871033221967, 275.7782546341398984 ) ) ;
#6589 = CIRCLE ( 'NONE', #19416, 3.399999999999985700 ) ;
#6590 = ORIENTED_EDGE ( 'NONE', *, *, #8759, .F. ) ;
#6591 = AXIS2_PLACEMENT_3D ( 'NONE', #1640, #15440, #5057 ) ;
#6592 = DIRECTION ( 'NONE',  ( -0.9999164797902015955, -6.965998958219364448E-18, 0.01292414190464157182 ) ) ;
#6593 = VECTOR ( 'NONE', #16228, 1000.000000000000000 ) ;
#6594 = ORIENTED_EDGE ( 'NONE', *, *, #12021, .T. ) ;
#6595 = ADVANCED_FACE ( 'NONE', ( #13030 ), #15174, .T. ) ;
#6596 = CARTESIAN_POINT ( 'NONE',  ( -12.01575389183062192, 182.4076787623453129, 322.7174846376778987 ) ) ;
#6597 = CARTESIAN_POINT ( 'NONE',  ( -90.04153719330230388, 72.97786998644573941, 61.59291218184642247 ) ) ;
#6598 = FACE_OUTER_BOUND ( 'NONE', #2839, .T. ) ;
#6599 = DIRECTION ( 'NONE',  ( 0.9726991065672921932, 0.2316562896908778701, -0.01384960395994898168 ) ) ;
#6600 = CARTESIAN_POINT ( 'NONE',  ( 44.03028354117878251, 168.0879242961143518, -75.31593853751020617 ) ) ;
#6601 = CARTESIAN_POINT ( 'NONE',  ( 13.03496960693103546, 190.3881593399657390, 320.8495494816559130 ) ) ;
#6602 = DIRECTION ( 'NONE',  ( -0.01292394549866731843, -0.005513023399720594006, -0.9999012842304693116 ) ) ;
#6603 = DIRECTION ( 'NONE',  ( 0.9999164797902017066, -5.258378535504111633E-16, -0.01292414190464131508 ) ) ;
#6604 = CONICAL_SURFACE ( 'NONE', #14336, 2.499999999999988010, 1.029744258676651425 ) ;
#6605 = CARTESIAN_POINT ( 'NONE',  ( -39.06508167816152621, 108.1171923551751917, 72.59136061629835979 ) ) ;
#6606 = AXIS2_PLACEMENT_3D ( 'NONE', #4238, #9304, #4344 ) ;
#6607 = EDGE_CURVE ( 'NONE', #18705, #4456, #1871, .T. ) ;
#6608 = EDGE_LOOP ( 'NONE', ( #11250, #13311, #13790 ) ) ;
#6609 = ADVANCED_FACE ( 'NONE', ( #22126, #14524 ), #19876, .T. ) ;
#6610 = DIRECTION ( 'NONE',  ( -0.009760756503428009989, 0.9999378516499564107, -0.005387065077611111891 ) ) ;
#6611 = CIRCLE ( 'NONE', #10645, 1.999999999999997780 ) ;
#6612 = DIRECTION ( 'NONE',  ( 0.000000000000000000, 0.000000000000000000, -1.000000000000000000 ) ) ;
#6613 = EDGE_CURVE ( 'NONE', #20796, #7407, #16201, .T. ) ;
#6614 = VERTEX_POINT ( 'NONE', #21706 ) ;
#6615 = LINE ( 'NONE', #4882, #13876 ) ;
#6616 = ORIENTED_EDGE ( 'NONE', *, *, #2503, .F. ) ;
#6617 = AXIS2_PLACEMENT_3D ( 'NONE', #2228, #3846, #9004 ) ;
#6618 = PRODUCT_DEFINITION_SHAPE ( 'NONE', 'NONE',  #22697 ) ;
#6619 = AXIS2_PLACEMENT_3D ( 'NONE', #6973, #22341, #6641 ) ;
#6620 = FACE_OUTER_BOUND ( 'NONE', #14710, .T. ) ;
#6621 = VECTOR ( 'NONE', #13172, 999.9999999999998863 ) ;
#6622 =( BOUNDED_CURVE ( )  B_SPLINE_CURVE ( 3, ( #12489, #14567, #7541, #540 ),
 .UNSPECIFIED., .F., .T. ) 
 B_SPLINE_CURVE_WITH_KNOTS ( ( 4, 4 ),
 ( 3.141592653589793560, 4.712388980384689674 ),
 .UNSPECIFIED. ) 
 CURVE ( )  GEOMETRIC_REPRESENTATION_ITEM ( )  RATIONAL_B_SPLINE_CURVE ( ( 1.000000000000000000, 0.8047378541243650485, 0.8047378541243650485, 1.000000000000000000 ) ) 
 REPRESENTATION_ITEM ( '' )  );
#6623 = ORIENTED_EDGE ( 'NONE', *, *, #9476, .T. ) ;
#6624 = DIRECTION ( 'NONE',  ( -0.000000000000000000, -1.000000000000000000, -0.000000000000000000 ) ) ;
#6625 = DIRECTION ( 'NONE',  ( 0.01292394549866738782, 0.005513023399720468239, 0.9999012842304692006 ) ) ;
#6626 = CARTESIAN_POINT ( 'NONE',  ( 13.46976562096918606, 144.2755497367511452, 275.9635810563158316 ) ) ;
#6627 = VECTOR ( 'NONE', #14447, 1000.000000000000114 ) ;
#6628 = ORIENTED_EDGE ( 'NONE', *, *, #18497, .F. ) ;
#6629 = CARTESIAN_POINT ( 'NONE',  ( 13.46024906002343968, 187.7400488015692588, 320.9343290008155805 ) ) ;
#6630 = EDGE_LOOP ( 'NONE', ( #2272, #246, #7193, #13783 ) ) ;
#6631 = CARTESIAN_POINT ( 'NONE',  ( -2.322807172541347498, 81.99999999999998579, -81.06750429846923112 ) ) ;
#6632 = VERTEX_POINT ( 'NONE', #18693 ) ;
#6633 = CARTESIAN_POINT ( 'NONE',  ( -64.99457118636311748, 170.0000000000008242, 0.8400692238025471159 ) ) ;
#6634 = DIRECTION ( 'NONE',  ( 0.1136178953597573593, -0.9935164314186355483, 0.004009283626633517415 ) ) ;
#6635 = CIRCLE ( 'NONE', #5142, 120.0000000000000000 ) ;
#6636 = ORIENTED_EDGE ( 'NONE', *, *, #2926, .F. ) ;
#6637 = LINE ( 'NONE', #16926, #22034 ) ;
#6638 = DIRECTION ( 'NONE',  ( 0.9934404589540163366, 0.1135548637187057675, -0.01346653032742958604 ) ) ;
#6639 = LINE ( 'NONE', #4908, #12834 ) ;
#6640 = VECTOR ( 'NONE', #6453, 999.9999999999998863 ) ;
#6641 = DIRECTION ( 'NONE',  ( 0.01292394549866695240, 0.005513023399718316314, 0.9999012842304693116 ) ) ;
#6642 = CARTESIAN_POINT ( 'NONE',  ( -4.915634481766264052, 156.2121883936867732, 81.74635178194236573 ) ) ;
#6643 = CARTESIAN_POINT ( 'NONE',  ( -8.312614011469616315, 69.99999999999998579, -95.45924547291811280 ) ) ;
#6644 = CARTESIAN_POINT ( 'NONE',  ( -41.42933370387425640, 166.0845032052916963, 276.3830402485593254 ) ) ;
#6645 = DIRECTION ( 'NONE',  ( -0.9934404589540162256, -0.1135548637187060589, 0.01346653032743275885 ) ) ;
#6646 = APPLICATION_PROTOCOL_DEFINITION ( 'draft international standard', 'automotive_design', 1998, #20253 ) ;
#6648 = ORIENTED_EDGE ( 'NONE', *, *, #21670, .F. ) ;
#6647 = ORIENTED_EDGE ( 'NONE', *, *, #5452, .T. ) ;
#6649 = CARTESIAN_POINT ( 'NONE',  ( -38.82295403925314758, 92.04141378167194887, 85.46747784716957597 ) ) ;
#6650 = EDGE_CURVE ( 'NONE', #11917, #168, #20561, .T. ) ;
#6651 = DIRECTION ( 'NONE',  ( -0.01292394549866741557, -0.005513023399720270480, -0.9999012842304693116 ) ) ;
#6652 = DIRECTION ( 'NONE',  ( -0.01292414190463827932, 0.000000000000000000, -0.9999164797902018176 ) ) ;
#6653 = DIRECTION ( 'NONE',  ( 0.9999164797902015955, 6.965998958219364448E-18, -0.01292414190464157182 ) ) ;
#6654 = DIRECTION ( 'NONE',  ( -7.125109674118361251E-05, 0.9999848031710253382, -0.005512562950849477644 ) ) ;
#6655 = ORIENTED_EDGE ( 'NONE', *, *, #6996, .T. ) ;
#6656 = LINE ( 'NONE', #5144, #3147 ) ;
#6657 = CARTESIAN_POINT ( 'NONE',  ( -44.49988481842637356, 152.0384941537814427, 275.3698588368105789 ) ) ;
#6658 = ORIENTED_EDGE ( 'NONE', *, *, #15764, .F. ) ;
#6659 = CARTESIAN_POINT ( 'NONE',  ( 50.20590380062862579, 109.5893650058224864, -44.82023758435901328 ) ) ;
#6660 = AXIS2_PLACEMENT_3D ( 'NONE', #10952, #19896, #2219 ) ;
#6661 = ORIENTED_EDGE ( 'NONE', *, *, #13297, .F. ) ;
#6662 = PLANE ( 'NONE',  #15473 ) ;
#6663 = LINE ( 'NONE', #2988, #14486 ) ;
#6664 = DIRECTION ( 'NONE',  ( -0.01292394549866695240, -0.005513023399718316314, -0.9999012842304693116 ) ) ;
#6665 = CARTESIAN_POINT ( 'NONE',  ( -18.87699466420334815, 140.4778767860208006, 87.01405127310822252 ) ) ;
#6666 = CARTESIAN_POINT ( 'NONE',  ( -50.93144557475185508, 189.6011917897851333, -71.74107005116499636 ) ) ;
#6667 = CARTESIAN_POINT ( 'NONE',  ( -44.54898248114630377, 168.6907664596094776, 35.18517999664061335 ) ) ;
#6668 = AXIS2_PLACEMENT_3D ( 'NONE', #8832, #8605, #14383 ) ;
#6669 = EDGE_CURVE ( 'NONE', #8505, #922, #19820, .T. ) ;
#6670 = ORIENTED_EDGE ( 'NONE', *, *, #13488, .F. ) ;
#6671 = FACE_OUTER_BOUND ( 'NONE', #22443, .T. ) ;
#6672 = ADVANCED_FACE ( 'NONE', ( #16252 ), #19756, .F. ) ;
#6673 = DIRECTION ( 'NONE',  ( -0.2120957809210262945, -0.9763012020921555401, 0.04302722985403674427 ) ) ;
#6674 = ORIENTED_EDGE ( 'NONE', *, *, #20353, .F. ) ;
#6675 = CIRCLE ( 'NONE', #12540, 10.00000000000000888 ) ;
#6676 = CARTESIAN_POINT ( 'NONE',  ( -90.11849266230689182, 87.42215604950109764, 51.14142411453754278 ) ) ;
#6678 = VERTEX_POINT ( 'NONE', #12780 ) ;
#6677 = VERTEX_POINT ( 'NONE', #13441 ) ;
#6679 = EDGE_CURVE ( 'NONE', #7165, #164, #401, .T. ) ;
#6680 = LINE ( 'NONE', #1311, #20591 ) ;
#6681 = ADVANCED_FACE ( 'NONE', ( #12903 ), #11171, .T. ) ;
#6682 = CARTESIAN_POINT ( 'NONE',  ( -41.52755568966412625, 166.0426042274538077, 268.7837904884077034 ) ) ;
#6683 = CARTESIAN_POINT ( 'NONE',  ( -33.37547251039675444, 92.26055912610783594, -80.91241141183517982 ) ) ;
#6684 = CARTESIAN_POINT ( 'NONE',  ( -1.163172771417702478, 87.00000000000001421, -89.99248318111824574 ) ) ;
#6685 = VECTOR ( 'NONE', #13678, 1000.000000000000000 ) ;
#6686 = CARTESIAN_POINT ( 'NONE',  ( -88.16245334966984615, 88.15582427846244684, 52.99867833143289886 ) ) ;
#6687 = FACE_OUTER_BOUND ( 'NONE', #17438, .T. ) ;
#6688 = AXIS2_PLACEMENT_3D ( 'NONE', #19610, #19945, #7561 ) ;
#6689 = VECTOR ( 'NONE', #21629, 1000.000000000000000 ) ;
#6690 = CARTESIAN_POINT ( 'NONE',  ( -51.18712128330030708, 189.4975170488156380, -90.54447405611476540 ) ) ;
#6691 = ORIENTED_EDGE ( 'NONE', *, *, #8691, .T. ) ;
#6692 = EDGE_CURVE ( 'NONE', #15161, #11316, #12877, .T. ) ;
#6693 = ORIENTED_EDGE ( 'NONE', *, *, #20555, .T. ) ;
#6694 = CARTESIAN_POINT ( 'NONE',  ( 19.46461987976676511, 177.6255169206013989, 113.1985551865116406 ) ) ;
#6695 = CARTESIAN_POINT ( 'NONE',  ( -73.00030478232707765, 95.66452290628956234, 82.28581592040848136 ) ) ;
#6696 = CARTESIAN_POINT ( 'NONE',  ( 92.46788464407293873, 79.04398536104962147, -28.62013883513330015 ) ) ;
#6697 = DIRECTION ( 'NONE',  ( -7.125109674161246868E-05, 0.9999848031710253382, -0.005512562950850155054 ) ) ;
#6698 = CARTESIAN_POINT ( 'NONE',  ( -10.32470579490272833, 146.5997690630838406, 277.1622549925964449 ) ) ;
#6699 = VERTEX_POINT ( 'NONE', #15288 ) ;
#6700 = CIRCLE ( 'NONE', #19532, 7.499999999999992006 ) ;
#6701 = DIRECTION ( 'NONE',  ( -0.8711556608166292071, -0.002768776501786239866, -0.4909991328951868184 ) ) ;
#6702 = VECTOR ( 'NONE', #3653, 1000.000000000000114 ) ;
#6703 = EDGE_CURVE ( 'NONE', #680, #8178, #4567, .T. ) ;
#6704 = EDGE_CURVE ( 'NONE', #9279, #20198, #1146, .T. ) ;
#6705 = DIRECTION ( 'NONE',  ( -0.01292394549866738782, -0.005513023399720468239, -0.9999012842304692006 ) ) ;
#6706 = ORIENTED_EDGE ( 'NONE', *, *, #21573, .F. ) ;
#6707 = AXIS2_PLACEMENT_3D ( 'NONE', #7901, #18474, #13429 ) ;
#6708 = VERTEX_POINT ( 'NONE', #15728 ) ;
#6709 = EDGE_CURVE ( 'NONE', #2480, #7828, #8818, .T. ) ;
#6710 = CARTESIAN_POINT ( 'NONE',  ( -58.43869058843797148, 126.9191314136037789, 167.6080500541861795 ) ) ;
#6712 = ORIENTED_EDGE ( 'NONE', *, *, #21939, .T. ) ;
#6711 = EDGE_LOOP ( 'NONE', ( #16225, #19008, #15681, #7851 ) ) ;
#6713 = CARTESIAN_POINT ( 'NONE',  ( 79.25753170385351609, 75.13519840835958519, -6.091774775480104154 ) ) ;
#6714 = DIRECTION ( 'NONE',  ( 0.9999164797902015955, 2.001050586450178695E-22, -0.01292414190464131335 ) ) ;
#6715 = CARTESIAN_POINT ( 'NONE',  ( 105.4775731789987105, 77.90269639574793814, -31.21677525025643263 ) ) ;
#6716 = CARTESIAN_POINT ( 'NONE',  ( -92.79593043952057485, 70.16589065052623653, -59.06731773122654516 ) ) ;
#6717 = EDGE_CURVE ( 'NONE', #4350, #12640, #10432, .T. ) ;
#6718 = CARTESIAN_POINT ( 'NONE',  ( 15.83726170982532544, 187.4852378640612756, 277.2946379115891204 ) ) ;
#6719 = ORIENTED_EDGE ( 'NONE', *, *, #19606, .F. ) ;
#6720 = DIRECTION ( 'NONE',  ( -0.01246513159389404414, -0.2641402835564772289, -0.9644037178988116299 ) ) ;
#6721 = CARTESIAN_POINT ( 'NONE',  ( 8.627475644446743530, 81.44091995301864984, -87.97989623083630306 ) ) ;
#6722 = CARTESIAN_POINT ( 'NONE',  ( 146.4999999999998863, 20.00000000000000000, -8.000000000002026823 ) ) ;
#6723 = CARTESIAN_POINT ( 'NONE',  ( -64.14035809025482138, 91.69347899441576999, 66.92892513032199986 ) ) ;
#6724 = CARTESIAN_POINT ( 'NONE',  ( -41.49220022125144425, 173.5884475113861924, 277.1425582878616183 ) ) ;
#6725 = CARTESIAN_POINT ( 'NONE',  ( 90.42410873942372973, 78.25489917908669213, -32.91867509261376057 ) ) ;
#6726 = EDGE_CURVE ( 'NONE', #1967, #15431, #15054, .T. ) ;
#6727 = FACE_OUTER_BOUND ( 'NONE', #20726, .T. ) ;
#6728 = FACE_OUTER_BOUND ( 'NONE', #12729, .T. ) ;
#6729 = ORIENTED_EDGE ( 'NONE', *, *, #20409, .T. ) ;
#6730 = FACE_OUTER_BOUND ( 'NONE', #2509, .T. ) ;
#6731 = EDGE_LOOP ( 'NONE', ( #15712, #7448, #14192, #15125 ) ) ;
#6732 = CIRCLE ( 'NONE', #8560, 9.000000000000001776 ) ;
#6733 = AXIS2_PLACEMENT_3D ( 'NONE', #3840, #1888, #12240 ) ;
#6734 = CARTESIAN_POINT ( 'NONE',  ( -4.067676644731632152, 70.07661102881314719, -81.29421751449218903 ) ) ;
#6735 = CARTESIAN_POINT ( 'NONE',  ( 39.36913080622081651, 72.00000000000000000, -87.51612159803863733 ) ) ;
#6736 = LINE ( 'NONE', #13762, #17944 ) ;
#6737 = DIRECTION ( 'NONE',  ( 0.01035335185279115042, 0.005513005182354825326, 0.9999312050732648283 ) ) ;
#6738 = EDGE_CURVE ( 'NONE', #10848, #5715, #6637, .T. ) ;
#6739 = EDGE_LOOP ( 'NONE', ( #206, #15187, #6296 ) ) ;
#6740 = EDGE_CURVE ( 'NONE', #592, #1880, #19117, .T. ) ;
#6741 = CARTESIAN_POINT ( 'NONE',  ( 12.61148133605082222, 188.1786184505010056, 320.9582656092828188 ) ) ;
#6742 = VECTOR ( 'NONE', #15870, 1000.000000000000000 ) ;
#6743 = CARTESIAN_POINT ( 'NONE',  ( 110.0057602926817424, 75.00002486432201465, -0.2635329904031751269 ) ) ;
#6744 = FACE_OUTER_BOUND ( 'NONE', #11586, .T. ) ;
#6745 = ORIENTED_EDGE ( 'NONE', *, *, #5425, .T. ) ;
#6746 = CYLINDRICAL_SURFACE ( 'NONE', #2251, 2.000000000000001332 ) ;
#6747 = AXIS2_PLACEMENT_3D ( 'NONE', #13294, #4533, #11905 ) ;
#6748 = CARTESIAN_POINT ( 'NONE',  ( -18.15695764360042119, 164.2346120007591992, 324.8972569404635351 ) ) ;
#6749 = CARTESIAN_POINT ( 'NONE',  ( 16.87037639224499586, 145.3228975761790025, 276.0538200153999924 ) ) ;
#6750 = CARTESIAN_POINT ( 'NONE',  ( 48.46580958134982353, 166.9169248112777666, 268.0158251802795917 ) ) ;
#6751 = CARTESIAN_POINT ( 'NONE',  ( 15.57127168073785128, 185.9592917570443262, 305.9563173247644272 ) ) ;
#6752 = CARTESIAN_POINT ( 'NONE',  ( 1.141353067861252457, 70.35701968572534781, -80.61740134152158532 ) ) ;
#6753 = ORIENTED_EDGE ( 'NONE', *, *, #20902, .F. ) ;
#6754 = CIRCLE ( 'NONE', #2382, 110.1134477342067157 ) ;
#6755 = CARTESIAN_POINT ( 'NONE',  ( 59.65144567478507298, 126.9191314136042479, 166.0817088952479139 ) ) ;
#6756 = CYLINDRICAL_SURFACE ( 'NONE', #1459, 95.00000000000000000 ) ;
#6757 = DIRECTION ( 'NONE',  ( 0.000000000000000000, 0.000000000000000000, 1.000000000000000000 ) ) ;
#6758 = B_SPLINE_CURVE_WITH_KNOTS ( 'NONE', 3,
 ( #8316, #4862, #9309, #2427, #16355, #4009 ),
 .UNSPECIFIED., .F., .F.,
 ( 4, 2, 4 ),
 ( 2.380730968575512647E-07, 0.002629065763328360464, 0.005257893453559862873 ),
 .UNSPECIFIED. ) ;
#6759 = CONTEXT_DEPENDENT_SHAPE_REPRESENTATION ( #20543, #12347 ) ;
#6760 = AXIS2_PLACEMENT_3D ( 'NONE', #8324, #15364, #10285 ) ;
#6761 = EDGE_LOOP ( 'NONE', ( #5986, #5388, #6778, #20852 ) ) ;
#6762 = VECTOR ( 'NONE', #17567, 999.9999999999998863 ) ;
#6763 = CARTESIAN_POINT ( 'NONE',  ( 13.85032138075246699, 137.5759562808229362, 104.3910387985238799 ) ) ;
#6764 = EDGE_CURVE ( 'NONE', #9560, #18446, #17108, .T. ) ;
#6765 = LINE ( 'NONE', #13787, #1150 ) ;
#6766 = CARTESIAN_POINT ( 'NONE',  ( 1.247179693797900502, 44.99899999999999523, 96.49194029975444664 ) ) ;
#6767 = ORIENTED_EDGE ( 'NONE', *, *, #12375, .F. ) ;
#6768 = CARTESIAN_POINT ( 'NONE',  ( 7.483496276596866004, 81.99999999999998579, -92.63956227386769626 ) ) ;
#6769 = CARTESIAN_POINT ( 'NONE',  ( 64.38126239552605057, 111.9218655255082382, -48.29061345977370934 ) ) ;
#6770 = ORIENTED_EDGE ( 'NONE', *, *, #11799, .F. ) ;
#6771 = CARTESIAN_POINT ( 'NONE',  ( -90.07495684815179970, 87.56539372961334777, 51.05391499655451781 ) ) ;
#6772 = VERTEX_POINT ( 'NONE', #13662 ) ;
#6773 = DIRECTION ( 'NONE',  ( 0.9999164797902015955, 0.000000000000000000, -0.01292414190464174703 ) ) ;
#6774 = CIRCLE ( 'NONE', #22519, 11.00000000000000178 ) ;
#6775 = CARTESIAN_POINT ( 'NONE',  ( -35.95309506732429128, 93.50464841319750064, -82.03286182426641915 ) ) ;
#6776 = DIRECTION ( 'NONE',  ( 0.9999164797902017066, 6.965998958219367529E-18, -0.01292414190464157182 ) ) ;
#6777 = DIRECTION ( 'NONE',  ( -7.125109674161257710E-05, 0.9999848031710252272, -0.005512562950850163727 ) ) ;
#6778 = ORIENTED_EDGE ( 'NONE', *, *, #10918, .F. ) ;
#6779 = PRODUCT_RELATED_PRODUCT_CATEGORY ( 'part', '', ( #20165 ) ) ;
#6780 = CYLINDRICAL_SURFACE ( 'NONE', #12785, 1.999999999999997780 ) ;
#6781 = CARTESIAN_POINT ( 'NONE',  ( 45.23671757199362986, 168.6025580852140138, 18.02358667753535926 ) ) ;
#6782 = EDGE_LOOP ( 'NONE', ( #10003, #13943, #12443, #3107 ) ) ;
#6783 = DIRECTION ( 'NONE',  ( 0.5089394657577702707, 0.004781488884709769391, 0.8607890319690654213 ) ) ;
#6784 = CARTESIAN_POINT ( 'NONE',  ( -90.02674258212728375, 88.67875473957917620, 52.55243696673224463 ) ) ;
#6785 = CARTESIAN_POINT ( 'NONE',  ( 4.188990710115612970, 166.7868399227302518, 324.0943093659811325 ) ) ;
#6786 = VECTOR ( 'NONE', #14608, 999.9999999999998863 ) ;
#6788 = VERTEX_POINT ( 'NONE', #1477 ) ;
#6787 = ORIENTED_EDGE ( 'NONE', *, *, #5102, .F. ) ;
#6789 = ORIENTED_EDGE ( 'NONE', *, *, #9747, .T. ) ;
#6790 = DIRECTION ( 'NONE',  ( -0.8711556608166292071, -0.002768776501786239432, -0.4909991328951867628 ) ) ;
#6791 = DIRECTION ( 'NONE',  ( -0.000000000000000000, -1.000000000000000000, -0.000000000000000000 ) ) ;
#6792 = DIRECTION ( 'NONE',  ( -0.9999164797902015955, -6.965998958219364448E-18, 0.01292414190464157182 ) ) ;
#6793 = ORIENTED_EDGE ( 'NONE', *, *, #10206, .F. ) ;
#6794 = DIRECTION ( 'NONE',  ( -0.01292394549866738608, -0.005513023399720699824, -0.9999012842304692006 ) ) ;
#6795 = ADVANCED_FACE ( 'NONE', ( #11827 ), #4905, .F. ) ;
#6796 = DIRECTION ( 'NONE',  ( -0.009760756503428008254, 0.9999378516499564107, -0.005387065077611006073 ) ) ;
#6797 = DIRECTION ( 'NONE',  ( -0.1296504907605104673, -0.005475273188900901117, -0.9915446392518421082 ) ) ;
#6798 = ORIENTED_EDGE ( 'NONE', *, *, #18266, .F. ) ;
#6799 = ORIENTED_EDGE ( 'NONE', *, *, #10085, .T. ) ;
#6800 = CARTESIAN_POINT ( 'NONE',  ( -7.125252400461968172, 188.3623996986441682, 276.8553851557323355 ) ) ;
#6801 = DIRECTION ( 'NONE',  ( -0.9999164797902017066, 0.000000000000000000, 0.01292414190463832269 ) ) ;
#6802 = DIRECTION ( 'NONE',  ( 1.387778780781445676E-14, 0.000000000000000000, -1.000000000000000000 ) ) ;
#6803 = CARTESIAN_POINT ( 'NONE',  ( 73.74384038452764401, 84.99999999999997158, -0.9531554654672952376 ) ) ;
#6804 = CYLINDRICAL_SURFACE ( 'NONE', #12135, 2.000000000000004441 ) ;
#6805 = CARTESIAN_POINT ( 'NONE',  ( 0.000000000000000000, 0.000000000000000000, 0.000000000000000000 ) ) ;
#6806 = LINE ( 'NONE', #13831, #14128 ) ;
#6807 = CIRCLE ( 'NONE', #3512, 10.00000000000000000 ) ;
#6808 = FACE_OUTER_BOUND ( 'NONE', #16337, .T. ) ;
#6809 = PRODUCT_DEFINITION_SHAPE ( 'NONE', 'NONE',  #22700 ) ;
#6810 = EDGE_CURVE ( 'NONE', #7475, #2837, #13295, .T. ) ;
#6811 = EDGE_LOOP ( 'NONE', ( #6512, #6845, #20504, #9867, #18369 ) ) ;
#6812 = CARTESIAN_POINT ( 'NONE',  ( -55.33804461215960657, 114.2193244133317904, 167.6379947637574617 ) ) ;
#6813 = EDGE_LOOP ( 'NONE', ( #10696, #3347, #4989 ) ) ;
#6814 = ORIENTED_EDGE ( 'NONE', *, *, #15793, .T. ) ;
#6815 = ORIENTED_EDGE ( 'NONE', *, *, #16561, .T. ) ;
#6816 = DIRECTION ( 'NONE',  ( -0.01292394549866728373, -0.005513023399720296501, -0.9999012842304693116 ) ) ;
#6817 = EDGE_CURVE ( 'NONE', #17658, #18467, #4807, .T. ) ;
#6818 = EDGE_LOOP ( 'NONE', ( #2426, #14125, #5383, #14158 ) ) ;
#6819 = DIRECTION ( 'NONE',  ( 1.362186893977296347E-14, 0.000000000000000000, -1.000000000000000000 ) ) ;
#6820 = DIRECTION ( 'NONE',  ( 7.125109674381880655E-05, -0.9999848031710253382, 0.005512562950849702291 ) ) ;
#6821 = ADVANCED_FACE ( 'NONE', ( #17560 ), #6746, .F. ) ;
#6822 = CYLINDRICAL_SURFACE ( 'NONE', #14459, 2.000000000000004885 ) ;
#6823 = DIRECTION ( 'NONE',  ( 0.01292394549866731843, 0.005513023399720594006, 0.9999012842304693116 ) ) ;
#6824 = EDGE_CURVE ( 'NONE', #11456, #16120, #12038, .T. ) ;
#6825 = SURFACE_STYLE_FILL_AREA ( #14204 ) ;
#6826 = CYLINDRICAL_SURFACE ( 'NONE', #1968, 1.999999999999997780 ) ;
#6827 = CARTESIAN_POINT ( 'NONE',  ( 11.96119988344894658, 187.7040126267789049, 304.8853073998464538 ) ) ;
#6828 = CARTESIAN_POINT ( 'NONE',  ( -50.95823800333778308, 189.5897628274961164, -73.81394971113282111 ) ) ;
#6829 = CARTESIAN_POINT ( 'NONE',  ( -57.91696284425325558, 114.3928197603287487, 162.9316086513573794 ) ) ;
#6830 = EDGE_LOOP ( 'NONE', ( #16097, #8532 ) ) ;
#6831 = B_SPLINE_CURVE_WITH_KNOTS ( 'NONE', 3,
 ( #13717, #8074, #11878, #13599 ),
 .UNSPECIFIED., .F., .F.,
 ( 4, 4 ),
 ( 0.000000000000000000, 0.001461243987308210755 ),
 .UNSPECIFIED. ) ;
#6832 = EDGE_CURVE ( 'NONE', #13967, #15481, #22436, .T. ) ;
#6833 = CARTESIAN_POINT ( 'NONE',  ( -9.872911121805453050, 164.2008282473921668, 81.76637977369325938 ) ) ;
#6834 = LINE ( 'NONE', #13640, #12882 ) ;
#6835 = ORIENTED_EDGE ( 'NONE', *, *, #5354, .F. ) ;
#6836 = CARTESIAN_POINT ( 'NONE',  ( -91.32251664931386870, 80.22595383786651269, -29.89762933574914783 ) ) ;
#6837 = ORIENTED_EDGE ( 'NONE', *, *, #18087, .F. ) ;
#6838 = EDGE_CURVE ( 'NONE', #13470, #1967, #17692, .T. ) ;
#6839 = CIRCLE ( 'NONE', #4992, 78.99999999999998579 ) ;
#6840 = CARTESIAN_POINT ( 'NONE',  ( 1.163172771417732010, 44.99899999999999523, 89.99248318111813205 ) ) ;
#6841 = CARTESIAN_POINT ( 'NONE',  ( 0.1821772113303683771, 327.3375983465229524, 315.3801061165882516 ) ) ;
#6842 = CARTESIAN_POINT ( 'NONE',  ( -104.8611102782643485, 69.99999999999998579, 33.22898942131119071 ) ) ;
#6843 = CARTESIAN_POINT ( 'NONE',  ( 17.16844361279197884, 146.4225787965282279, 277.8094805302229702 ) ) ;
#6844 = EDGE_CURVE ( 'NONE', #13521, #10577, #1174, .T. ) ;
#6845 = ORIENTED_EDGE ( 'NONE', *, *, #21257, .T. ) ;
#6846 = PLANE ( 'NONE',  #2917 ) ;
#6847 = EDGE_LOOP ( 'NONE', ( #9285, #17656 ) ) ;
#6848 = LINE ( 'NONE', #13869, #13008 ) ;
#6849 = CARTESIAN_POINT ( 'NONE',  ( 108.2664294940537530, 76.72841911532559322, -19.58316954391773734 ) ) ;
#6850 = CARTESIAN_POINT ( 'NONE',  ( 109.9781218937930589, 75.08416348859606160, 3.222660468417843482 ) ) ;
#6851 = DIRECTION ( 'NONE',  ( 0.9999164797902015955, 6.965998958219364448E-18, -0.01292414190464157182 ) ) ;
#6852 = VERTEX_POINT ( 'NONE', #8795 ) ;
#6853 = DIRECTION ( 'NONE',  ( 0.9999164797902015955, 6.965998958219364448E-18, -0.01292414190464157182 ) ) ;
#6854 = CARTESIAN_POINT ( 'NONE',  ( -91.73057767193260759, 77.20311952920093290, 31.31041951043025406 ) ) ;
#6855 = PLANE ( 'NONE',  #9527 ) ;
#6856 = CARTESIAN_POINT ( 'NONE',  ( 163.9999999999998295, 19.17157287525381193, 8.000000000002229328 ) ) ;
#6857 = CARTESIAN_POINT ( 'NONE',  ( 17.34172197772754132, 185.0087168425970106, 321.6195380205137440 ) ) ;
#6858 = EDGE_CURVE ( 'NONE', #379, #4610, #7089, .T. ) ;
#6859 = LINE ( 'NONE', #13884, #6762 ) ;
#6860 = CARTESIAN_POINT ( 'NONE',  ( 51.99565694909076541, 169.9999999999999716, -0.6720553790413538175 ) ) ;
#6861 = AXIS2_PLACEMENT_3D ( 'NONE', #8304, #20584, #16943 ) ;
#6862 = DIRECTION ( 'NONE',  ( 0.000000000000000000, -0.9455185755993167351, 0.3255681544571568109 ) ) ;
#6863 = DIRECTION ( 'NONE',  ( 0.9999164797902017066, 2.001050586450180576E-22, -0.01292414190464044946 ) ) ;
#6864 = CARTESIAN_POINT ( 'NONE',  ( 1.236893267138826732E-14, 29.00000000000000355, 101.0000000000000000 ) ) ;
#6866 = VERTEX_POINT ( 'NONE', #8578 ) ;
#6865 = ORIENTED_EDGE ( 'NONE', *, *, #10366, .T. ) ;
#6867 = CARTESIAN_POINT ( 'NONE',  ( -37.28121903586303887, 92.86731729159741633, 84.62157808538474058 ) ) ;
#6868 = DIRECTION ( 'NONE',  ( 7.125109674364534776E-05, -0.9999848031710252272, 0.005512562950849704893 ) ) ;
#6869 = EDGE_CURVE ( 'NONE', #4488, #21806, #9609, .T. ) ;
#6870 = DIRECTION ( 'NONE',  ( -7.125109674243555432E-05, 0.9999848031710253382, -0.005512562950850175003 ) ) ;
#6871 = DIRECTION ( 'NONE',  ( -7.125109674403276030E-05, 0.9999848031710252272, -0.005512562950848280685 ) ) ;
#6872 = ORIENTED_EDGE ( 'NONE', *, *, #155, .F. ) ;
#6873 = DIRECTION ( 'NONE',  ( -0.01292394549866727679, -0.005513023399720742325, -0.9999012842304692006 ) ) ;
#6874 = CARTESIAN_POINT ( 'NONE',  ( 146.5000000000000000, 1.999999999999998224, -2.025191382850354537E-12 ) ) ;
#6875 = ORIENTED_EDGE ( 'NONE', *, *, #21670, .T. ) ;
#6876 = CARTESIAN_POINT ( 'NONE',  ( 47.42524840967396216, 108.3817487785543108, -44.77763872393808953 ) ) ;
#6877 = ORIENTED_EDGE ( 'NONE', *, *, #16268, .T. ) ;
#6878 = DIRECTION ( 'NONE',  ( -0.7944560844389304544, 0.000000000000000000, -0.6073216033519334145 ) ) ;
#6879 = DIRECTION ( 'NONE',  ( -0.01292414190464131335, -1.902755938799530239E-22, -0.9999164797902015955 ) ) ;
#6880 = CARTESIAN_POINT ( 'NONE',  ( -55.33804461215960657, 114.2193244133317904, 167.6379947637574617 ) ) ;
#6881 = CYLINDRICAL_SURFACE ( 'NONE', #2993, 2.000000000000004885 ) ;
#6882 = AXIS2_PLACEMENT_3D ( 'NONE', #7228, #14256, #12529 ) ;
#6883 = VERTEX_POINT ( 'NONE', #22561 ) ;
#6884 = CARTESIAN_POINT ( 'NONE',  ( 8.732865712828665750, 190.3249964942741883, 274.4707185275763095 ) ) ;
#6885 = CARTESIAN_POINT ( 'NONE',  ( -54.52327687265815825, 18.00000000000000355, -111.3697098814011923 ) ) ;
#6886 = ORIENTED_EDGE ( 'NONE', *, *, #15184, .T. ) ;
#6887 = CARTESIAN_POINT ( 'NONE',  ( 20.78937598082199756, 168.6311526966014185, 310.6889741221851295 ) ) ;
#6888 = EDGE_CURVE ( 'NONE', #5416, #13498, #20864, .T. ) ;
#6889 = EDGE_CURVE ( 'NONE', #16785, #10445, #1704, .T. ) ;
#6890 = VERTEX_POINT ( 'NONE', #16416 ) ;
#6891 = AXIS2_PLACEMENT_3D ( 'NONE', #18409, #11062, #11178 ) ;
#6892 = CARTESIAN_POINT ( 'NONE',  ( 79.99331838321626265, 102.0000000000000000, -1.033931352371318058 ) ) ;
#6893 = CARTESIAN_POINT ( 'NONE',  ( -88.16993261600009646, 88.76241539977888806, 52.31541104021305699 ) ) ;
#6894 = LINE ( 'NONE', #13916, #3080 ) ;
#6896 = EDGE_LOOP ( 'NONE', ( #6712, #15947, #20143, #3890 ) ) ;
#6895 = ORIENTED_EDGE ( 'NONE', *, *, #1400, .F. ) ;
#6897 = CIRCLE ( 'NONE', #19725, 1.999999999999998446 ) ;
#6898 = ORIENTED_EDGE ( 'NONE', *, *, #16589, .F. ) ;
#6899 = CARTESIAN_POINT ( 'NONE',  ( -8.330024601187750122, 185.3742117612894447, 323.2535488253523681 ) ) ;
#6900 = B_SPLINE_CURVE_WITH_KNOTS ( 'NONE', 3,
 ( #9350, #16388, #11200, #6129, #6020, #5898, #12934, #21839, #2459, #13056, #13270, #11542 ),
 .UNSPECIFIED., .F., .F.,
 ( 4, 2, 2, 2, 2, 4 ),
 ( 0.04309441970742561301, 0.05230155063785107278, 0.06150868156827653255, 0.06611224703348925202, 0.07071581249870198538, 0.07992294342912742433 ),
 .UNSPECIFIED. ) ;
#6901 = DIRECTION ( 'NONE',  ( 0.9999164797902015955, 6.965998958219364448E-18, -0.01292414190464157182 ) ) ;
#6902 = CARTESIAN_POINT ( 'NONE',  ( -30.68998116395940912, 91.18377996386419682, -79.89680297002404075 ) ) ;
#6903 =( NAMED_UNIT ( * ) SI_UNIT ( $, .STERADIAN. ) SOLID_ANGLE_UNIT ( ) );
#6904 = CARTESIAN_POINT ( 'NONE',  ( 82.49079974960680772, 75.10299918630330751, -5.493043209074147448 ) ) ;
#6905 = PLANE ( 'NONE',  #3800 ) ;
#6906 = ORIENTED_EDGE ( 'NONE', *, *, #18154, .F. ) ;
#6907 = VERTEX_POINT ( 'NONE', #7203 ) ;
#6908 = EDGE_LOOP ( 'NONE', ( #10585, #22520, #10678, #3911 ) ) ;
#6909 = DIRECTION ( 'NONE',  ( -0.01292394549866728373, -0.005513023399720296501, -0.9999012842304693116 ) ) ;
#6910 = CARTESIAN_POINT ( 'NONE',  ( 24.53513420042494886, 169.1064450938641244, 322.3183935679231240 ) ) ;
#6911 = CARTESIAN_POINT ( 'NONE',  ( -9.008850598706597879, 165.4223666312992691, 76.74798293798586712 ) ) ;
#6912 = CARTESIAN_POINT ( 'NONE',  ( -28.23059182152518787, 324.0912873339099178, 316.1123282797007050 ) ) ;
#6913 = AXIS2_PLACEMENT_3D ( 'NONE', #9576, #14772, #16608 ) ;
#6914 = CARTESIAN_POINT ( 'NONE',  ( -92.46042328379806463, 77.12912189496637438, 29.19741020490883088 ) ) ;
#6915 = VECTOR ( 'NONE', #18966, 1000.000000000000000 ) ;
#6916 = LINE ( 'NONE', #13937, #15976 ) ;
#6917 = CARTESIAN_POINT ( 'NONE',  ( 0.000000000000000000, 37.00000000000000711, -83.99999999999998579 ) ) ;
#6918 = EDGE_CURVE ( 'NONE', #17451, #16857, #12816, .T. ) ;
#6919 = CARTESIAN_POINT ( 'NONE',  ( 0.000000000000000000, 29.00000000000000355, 0.000000000000000000 ) ) ;
#6920 = ORIENTED_EDGE ( 'NONE', *, *, #19587, .F. ) ;
#6921 = ORIENTED_EDGE ( 'NONE', *, *, #14189, .F. ) ;
#6922 = FACE_OUTER_BOUND ( 'NONE', #17862, .T. ) ;
#6923 = EDGE_LOOP ( 'NONE', ( #11376, #9479, #8256, #19866 ) ) ;
#6924 = CARTESIAN_POINT ( 'NONE',  ( 18.69536052806380511, 189.4444907833431273, -101.0667417618365107 ) ) ;
#6925 = CARTESIAN_POINT ( 'NONE',  ( -9.912705577010312730E-16, 1.999999999999998224, -9.999999999999994671 ) ) ;
#6926 = VECTOR ( 'NONE', #13550, 1000.000000000000000 ) ;
#6927 = CARTESIAN_POINT ( 'NONE',  ( -58.31448377536617755, 138.9208812252028622, 167.8907811906817074 ) ) ;
#6928 = FACE_OUTER_BOUND ( 'NONE', #10723, .T. ) ;
#6929 = EDGE_CURVE ( 'NONE', #6678, #15431, #15598, .T. ) ;
#6930 = CARTESIAN_POINT ( 'NONE',  ( 1.364375150383346228E-14, 45.00000000000000000, -9.836439021161248541E-15 ) ) ;
#6931 = CARTESIAN_POINT ( 'NONE',  ( -89.94862617306016261, 81.58347563513834189, 79.55911641354585129 ) ) ;
#6932 = CARTESIAN_POINT ( 'NONE',  ( 85.81624039914329671, 75.02539222853825152, -3.313852530756491888 ) ) ;
#6933 = CARTESIAN_POINT ( 'NONE',  ( 12.85290515736519090, 190.4809086768308362, 307.8507757859636627 ) ) ;
#6934 = CARTESIAN_POINT ( 'NONE',  ( 3.807734317907725430, 166.6242057324384689, 294.5972214811819754 ) ) ;
#6935 = CARTESIAN_POINT ( 'NONE',  ( -11.19281454843939194, 155.5569384583423300, 101.2152518466410243 ) ) ;
#6936 = VERTEX_POINT ( 'NONE', #12394 ) ;
#6937 = AXIS2_PLACEMENT_3D ( 'NONE', #8320, #10586, #12435 ) ;
#6938 = PRESENTATION_LAYER_ASSIGNMENT (  '', '', ( #10620 ) ) ;
#6939 = LINE ( 'NONE', #10291, #9175 ) ;
#6940 = CARTESIAN_POINT ( 'NONE',  ( -9.891059059079783111, 187.9599303772540964, 308.1469373984825211 ) ) ;
#6941 = AXIS2_PLACEMENT_3D ( 'NONE', #4571, #1024, #15397 ) ;
#6942 = ORIENTED_EDGE ( 'NONE', *, *, #19791, .F. ) ;
#6943 = LINE ( 'NONE', #22323, #6170 ) ;
#6944 = EDGE_CURVE ( 'NONE', #20064, #10751, #13276, .T. ) ;
#6945 = VERTEX_POINT ( 'NONE', #8920 ) ;
#6946 = EDGE_CURVE ( 'NONE', #2340, #10951, #14474, .T. ) ;
#6947 = CARTESIAN_POINT ( 'NONE',  ( -72.65963751957909267, 87.42236182341126494, 69.77244766351077487 ) ) ;
#6948 = B_SPLINE_CURVE_WITH_KNOTS ( 'NONE', 3,
 ( #9736, #14807, #9484, #7884, #997, #9832, #13183, #2484, #14923, #20275, #21754, #7984, #18666, #20045 ),
 .UNSPECIFIED., .F., .F.,
 ( 4, 2, 2, 2, 2, 2, 4 ),
 ( 0.000000000000000000, 0.0003932600017084012011, 0.0007865200034168024022, 0.001179780005125203712, 0.001573040006833604804, 0.002359560010250444286, 0.003146080013667283768 ),
 .UNSPECIFIED. ) ;
#6949 = CARTESIAN_POINT ( 'NONE',  ( 58.87479767622038906, 143.5880916635284166, 105.9939182712553105 ) ) ;
#6950 = AXIS2_PLACEMENT_3D ( 'NONE', #5004, #13986, #4773 ) ;
#6951 = FACE_OUTER_BOUND ( 'NONE', #5315, .T. ) ;
#6952 = VECTOR ( 'NONE', #7739, 999.9999999999998863 ) ;
#6953 = FILL_AREA_STYLE_COLOUR ( '', #6185 ) ;
#6954 = EDGE_CURVE ( 'NONE', #2665, #15942, #16227, .T. ) ;
#6955 = CARTESIAN_POINT ( 'NONE',  ( 16.44176152114187417, 145.9028759403760205, 276.6200799972182836 ) ) ;
#6956 = ORIENTED_EDGE ( 'NONE', *, *, #21695, .F. ) ;
#6957 = CYLINDRICAL_SURFACE ( 'NONE', #5093, 2.000000000000001776 ) ;
#6958 = ORIENTED_EDGE ( 'NONE', *, *, #17625, .F. ) ;
#6959 = VERTEX_POINT ( 'NONE', #18019 ) ;
#6960 = DIRECTION ( 'NONE',  ( -0.01292394549866632963, -0.005513023399716958026, -0.9999012842304692006 ) ) ;
#6961 = CARTESIAN_POINT ( 'NONE',  ( 14.14167086503323034, 113.6998737626107641, 126.9321988120954643 ) ) ;
#6962 = EDGE_CURVE ( 'NONE', #10899, #20552, #16951, .T. ) ;
#6963 = CARTESIAN_POINT ( 'NONE',  ( 110.0024317885484635, 75.02128446332422129, 0.8997087025338614819 ) ) ;
#6964 = ORIENTED_EDGE ( 'NONE', *, *, #8099, .F. ) ;
#6965 = CARTESIAN_POINT ( 'NONE',  ( 106.1636641531657972, 79.04398536104962147, -28.79715981783310497 ) ) ;
#6966 = AXIS2_PLACEMENT_3D ( 'NONE', #6287, #11573, #9623 ) ;
#6967 = DIRECTION ( 'NONE',  ( 7.125109674160325297E-05, -0.9999848031710252272, 0.005512562950849327591 ) ) ;
#6968 = ORIENTED_EDGE ( 'NONE', *, *, #5883, .T. ) ;
#6969 = DIRECTION ( 'NONE',  ( -0.9934404589540162256, -0.1135548637187055315, 0.01346653032743023309 ) ) ;
#6970 = ORIENTED_EDGE ( 'NONE', *, *, #22112, .F. ) ;
#6971 = CARTESIAN_POINT ( 'NONE',  ( -91.12451015595505055, 77.41163679146356458, 31.64200013680033052 ) ) ;
#6972 = DIRECTION ( 'NONE',  ( 0.01292394549866728373, 0.005513023399720296501, 0.9999012842304693116 ) ) ;
#6973 = CARTESIAN_POINT ( 'NONE',  ( -50.59277787925817194, 113.4706157781613598, -45.53898929444733312 ) ) ;
#6974 = VECTOR ( 'NONE', #9813, 999.9999999999998863 ) ;
#6975 = AXIS2_PLACEMENT_3D ( 'NONE', #19435, #22620, #5305 ) ;
#6976 = CARTESIAN_POINT ( 'NONE',  ( 18.78219705323197886, 183.8529737559827311, 320.0839512733973038 ) ) ;
#6977 = EDGE_CURVE ( 'NONE', #4119, #8602, #16315, .T. ) ;
#6978 = CARTESIAN_POINT ( 'NONE',  ( -45.36474727608069912, 165.8559883853732515, 234.9810740996818197 ) ) ;
#6979 = CARTESIAN_POINT ( 'NONE',  ( -65.56790548363530036, 144.7550503794368524, -43.51772385068294113 ) ) ;
#6980 = CARTESIAN_POINT ( 'NONE',  ( 58.10057221494500368, 126.2575686056377435, 46.09355478759161429 ) ) ;
#6981 = DIRECTION ( 'NONE',  ( 0.9999464000778708339, 1.417269118681874529E-05, -0.01035358732233823860 ) ) ;
#6982 = CARTESIAN_POINT ( 'NONE',  ( -10.81153106956454479, 81.64473548815914228, -89.75216824834804186 ) ) ;
#6983 = CIRCLE ( 'NONE', #2950, 4.500000000000006217 ) ;
#6984 = DIRECTION ( 'NONE',  ( 0.9934404589540162256, 0.1135548637187060589, -0.01346653032743021922 ) ) ;
#6985 = LINE ( 'NONE', #4921, #1602 ) ;
#6986 = DIRECTION ( 'NONE',  ( 0.8504393858994485633, -0.002839416958724378954, -0.5260653843604455870 ) ) ;
#6987 = CARTESIAN_POINT ( 'NONE',  ( 51.42288047930752271, 166.7281037598372961, 233.7252641129099970 ) ) ;
#6988 = EDGE_CURVE ( 'NONE', #126, #20005, #7402, .T. ) ;
#6989 = AXIS2_PLACEMENT_3D ( 'NONE', #4026, #16369, #21485 ) ;
#6990 = ORIENTED_EDGE ( 'NONE', *, *, #2365, .F. ) ;
#6991 = DIRECTION ( 'NONE',  ( 0.01292394549866738782, 0.005513023399720468239, 0.9999012842304692006 ) ) ;
#6992 = PRODUCT_DEFINITION_SHAPE ( 'NONE', 'NONE',  #22682 ) ;
#6993 = CARTESIAN_POINT ( 'NONE',  ( -49.75352177949782373, 112.0038634918761602, -43.54155237634173403 ) ) ;
#6994 = CIRCLE ( 'NONE', #12156, 10.99999999999999289 ) ;
#6995 = VERTEX_POINT ( 'NONE', #6284 ) ;
#6996 = EDGE_CURVE ( 'NONE', #1331, #11181, #2727, .T. ) ;
#6997 = CARTESIAN_POINT ( 'NONE',  ( 49.42508136925437867, 108.3817487785542966, -44.80348700774737836 ) ) ;
#6998 = ORIENTED_EDGE ( 'NONE', *, *, #10083, .F. ) ;
#6999 = CARTESIAN_POINT ( 'NONE',  ( -66.42677970909001317, 189.3893605493459233, -109.9672025422466959 ) ) ;
#7000 = CIRCLE ( 'NONE', #7351, 4.199999999999997513 ) ;
#7001 = CARTESIAN_POINT ( 'NONE',  ( -9.646142312030677957, 70.14698466122825948, -93.71525484045396581 ) ) ;
#7002 = DIRECTION ( 'NONE',  ( -0.4397038457472354778, 0.000000000000000000, -0.8981428216242066664 ) ) ;
#7003 = CARTESIAN_POINT ( 'NONE',  ( -13.92525281995234820, 325.7770340667113942, 328.4523304068723064 ) ) ;
#7004 = DIRECTION ( 'NONE',  ( 0.9999164797902015955, 2.457859219970326020E-15, -0.01292414190464043211 ) ) ;
#7005 = CARTESIAN_POINT ( 'NONE',  ( 44.31784132852413194, 168.2105890667581605, -53.06813496338226344 ) ) ;
#7006 = DIRECTION ( 'NONE',  ( 0.01292394549866731669, 0.005513023399720593139, 0.9999012842304692006 ) ) ;
#7007 = VECTOR ( 'NONE', #19484, 1000.000000000000114 ) ;
#7008 = ORIENTED_EDGE ( 'NONE', *, *, #220, .T. ) ;
#7009 = CARTESIAN_POINT ( 'NONE',  ( 20.88447817041588195, 168.6717208494654017, 318.0468511356601766 ) ) ;
#7010 = ADVANCED_FACE ( 'NONE', ( #9838 ), #15120, .T. ) ;
#7011 = CARTESIAN_POINT ( 'NONE',  ( -16.82948163695635557, 175.4987477760657839, 90.67711988367965148 ) ) ;
#7012 = ORIENTED_EDGE ( 'NONE', *, *, #1069, .T. ) ;
#7013 = CARTESIAN_POINT ( 'NONE',  ( -8.580473483290075976, 81.99999999999994316, -95.10893838946510925 ) ) ;
#7014 = VECTOR ( 'NONE', #21165, 1000.000000000000000 ) ;
#7015 = CARTESIAN_POINT ( 'NONE',  ( -90.02889123584817810, 87.66185544671367325, 50.99467065406356880 ) ) ;
#7016 =( GEOMETRIC_REPRESENTATION_CONTEXT ( 3 ) GLOBAL_UNCERTAINTY_ASSIGNED_CONTEXT ( ( #21677 ) ) GLOBAL_UNIT_ASSIGNED_CONTEXT ( ( #19171, #14026, #12649 ) ) REPRESENTATION_CONTEXT ( 'NONE', 'WORKASPACE' ) );
#7017 = CIRCLE ( 'NONE', #12528, 9.000000000000001776 ) ;
#7018 = EDGE_LOOP ( 'NONE', ( #2306, #6990, #2135 ) ) ;
#7019 = ORIENTED_EDGE ( 'NONE', *, *, #5108, .T. ) ;
#7020 = DIRECTION ( 'NONE',  ( 0.01292394549866733404, 0.005513023399720420534, 0.9999012842304693116 ) ) ;
#7021 = AXIS2_PLACEMENT_3D ( 'NONE', #10098, #20646, #11938 ) ;
#7022 = CARTESIAN_POINT ( 'NONE',  ( -36.55288090549052527, 94.02752048664899576, 83.45186405039063970 ) ) ;
#7023 = EDGE_LOOP ( 'NONE', ( #8643, #845, #14519, #16532, #7504, #14191, #901, #10628, #16292, #20234, #7765, #20073 ) ) ;
#7024 = CARTESIAN_POINT ( 'NONE',  ( -3.778596073675196454, 158.7497035399487402, 299.7391867095999487 ) ) ;
#7025 = CARTESIAN_POINT ( 'NONE',  ( 82.19586818426773789, 75.11053174630316676, -5.645930764600690210 ) ) ;
#7026 = DIRECTION ( 'NONE',  ( -0.1296504907605101897, -0.005475273188901851745, -0.9915446392518422192 ) ) ;
#7027 = ORIENTED_EDGE ( 'NONE', *, *, #6889, .F. ) ;
#7028 = ADVANCED_FACE ( 'NONE', ( #14693, #9492, #4204, #8117 ), #13308, .F. ) ;
#7029 = ORIENTED_EDGE ( 'NONE', *, *, #17100, .T. ) ;
#7030 = ADVANCED_FACE ( 'NONE', ( #7989 ), #2492, .F. ) ;
#7031 = LINE ( 'NONE', #5179, #17778 ) ;
#7032 = CARTESIAN_POINT ( 'NONE',  ( -78.73812145396803430, 75.12795917139310120, -3.912027923891130410 ) ) ;
#7033 = CARTESIAN_POINT ( 'NONE',  ( -9.855893760047319319, 165.1672551789314127, 320.7685678595336185 ) ) ;
#7034 = VECTOR ( 'NONE', #15172, 1000.000000000000000 ) ;
#7035 = CIRCLE ( 'NONE', #18756, 93.00000000000001421 ) ;
#7036 = CARTESIAN_POINT ( 'NONE',  ( -10.92725181965738024, 335.2393912496561938, 320.3606194292975147 ) ) ;
#7037 = ORIENTED_EDGE ( 'NONE', *, *, #11529, .F. ) ;
#7038 = CARTESIAN_POINT ( 'NONE',  ( -36.36981320942769003, 93.68077895625195595, -82.19051798928661867 ) ) ;
#7039 = DIRECTION ( 'NONE',  ( 0.01292394549866738782, 0.005513023399720468239, 0.9999012842304692006 ) ) ;
#7040 = CARTESIAN_POINT ( 'NONE',  ( -50.77397788485747299, 114.2585728760336394, 165.3737801152228712 ) ) ;
#7041 = ORIENTED_EDGE ( 'NONE', *, *, #14627, .F. ) ;
#7042 = AXIS2_PLACEMENT_3D ( 'NONE', #13481, #12212, #1744 ) ;
#7043 = CARTESIAN_POINT ( 'NONE',  ( 7.145902869757795983, 81.99999999999998579, -93.45069977196735067 ) ) ;
#7044 = ORIENTED_EDGE ( 'NONE', *, *, #17432, .T. ) ;
#7045 = ORIENTED_EDGE ( 'NONE', *, *, #5413, .F. ) ;
#7046 = CARTESIAN_POINT ( 'NONE',  ( 16.51658783711441814, 187.6325752588389832, 308.9821593705616465 ) ) ;
#7047 = CIRCLE ( 'NONE', #21351, 2.999999999999988898 ) ;
#7048 = VERTEX_POINT ( 'NONE', #779 ) ;
#7049 = LINE ( 'NONE', #21391, #19378 ) ;
#7050 = DIRECTION ( 'NONE',  ( -9.912705577010319386E-17, 0.000000000000000000, -1.000000000000000000 ) ) ;
#7051 = CARTESIAN_POINT ( 'NONE',  ( 3.833582208905060185, 166.6352317792379267, 296.5970240496429255 ) ) ;
#7052 = LINE ( 'NONE', #15581, #4531 ) ;
#7053 = EDGE_CURVE ( 'NONE', #5578, #18403, #3725, .T. ) ;
#7054 = DIRECTION ( 'NONE',  ( 0.01292414190464131508, 0.000000000000000000, 0.9999164797902017066 ) ) ;
#7055 = CIRCLE ( 'NONE', #12951, 5.099999999999994316 ) ;
#7056 = VERTEX_POINT ( 'NONE', #2610 ) ;
#7057 = CARTESIAN_POINT ( 'NONE',  ( 86.19166422048218124, 75.00269207195897536, -1.933333109913331738 ) ) ;
#7058 = CARTESIAN_POINT ( 'NONE',  ( 19.12444408178815891, 184.6244491382951480, 311.5251542095542732 ) ) ;
#7059 = CARTESIAN_POINT ( 'NONE',  ( 92.35175351209242933, 79.88298967448075416, 28.93780754488613738 ) ) ;
#7060 = FACE_OUTER_BOUND ( 'NONE', #16627, .T. ) ;
#7061 = VERTEX_POINT ( 'NONE', #11232 ) ;
#7062 = CIRCLE ( 'NONE', #10388, 6.000000000000003553 ) ;
#7063 = AXIS2_PLACEMENT_3D ( 'NONE', #14927, #18790, #20153 ) ;
#7064 = DIRECTION ( 'NONE',  ( -2.459148776293844314E-24, 1.000000000000000000, -1.902597020224326827E-22 ) ) ;
#7065 = FACE_OUTER_BOUND ( 'NONE', #10869, .T. ) ;
#7066 = ORIENTED_EDGE ( 'NONE', *, *, #4914, .F. ) ;
#7067 = CARTESIAN_POINT ( 'NONE',  ( -93.17671387018313567, 79.04398536104955042, -26.22064129356662576 ) ) ;
#7068 = ORIENTED_EDGE ( 'NONE', *, *, #19159, .F. ) ;
#7069 = CIRCLE ( 'NONE', #12226, 77.00000000000002842 ) ;
#7070 = LINE ( 'NONE', #19356, #9924 ) ;
#7071 = DIRECTION ( 'NONE',  ( -0.01292394549866741557, -0.005513023399720270480, -0.9999012842304693116 ) ) ;
#7072 = CIRCLE ( 'NONE', #11864, 3.399999999999986144 ) ;
#7073 = ORIENTED_EDGE ( 'NONE', *, *, #13722, .F. ) ;
#7074 = EDGE_CURVE ( 'NONE', #8665, #4350, #13190, .T. ) ;
#7075 = AXIS2_PLACEMENT_3D ( 'NONE', #2130, #15713, #17544 ) ;
#7076 = CARTESIAN_POINT ( 'NONE',  ( 1.440275352545798748, 177.6144908738019694, 111.4313871723342544 ) ) ;
#7077 = LINE ( 'NONE', #17789, #3209 ) ;
#7078 = DIRECTION ( 'NONE',  ( 0.01292414190464131335, 0.000000000000000000, 0.9999164797902017066 ) ) ;
#7079 = ORIENTED_EDGE ( 'NONE', *, *, #18193, .F. ) ;
#7080 = CARTESIAN_POINT ( 'NONE',  ( 12.27551321668195428, 188.3303010113484675, 320.9534237498031644 ) ) ;
#7081 = ORIENTED_EDGE ( 'NONE', *, *, #17287, .T. ) ;
#7082 = LINE ( 'NONE', #10766, #16684 ) ;
#7083 = EDGE_CURVE ( 'NONE', #16665, #13967, #14813, .T. ) ;
#7084 = CARTESIAN_POINT ( 'NONE',  ( 71.26616241777607286, 92.22173151023523019, 83.79227730723269474 ) ) ;
#7085 = DIRECTION ( 'NONE',  ( -0.9999164797902015955, -4.476705744456278510E-15, 0.01292414190464144692 ) ) ;
#7086 = DIRECTION ( 'NONE',  ( 7.125109674160325297E-05, -0.9999848031710253382, 0.005512562950849327591 ) ) ;
#7087 = AXIS2_PLACEMENT_3D ( 'NONE', #13268, #1082, #10035 ) ;
#7088 = ORIENTED_EDGE ( 'NONE', *, *, #17310, .T. ) ;
#7089 = LINE ( 'NONE', #10202, #18415 ) ;
#7090 = DIRECTION ( 'NONE',  ( 7.125109674161238737E-05, -0.9999848031710253382, 0.005512562950850163727 ) ) ;
#7091 = CARTESIAN_POINT ( 'NONE',  ( -5.774671379064696630, 326.6239185723279661, 307.3367782756131419 ) ) ;
#7092 = SHAPE_REPRESENTATION ( 'Square Thread Nut', ( #6292 ), #12539 ) ;
#7093 = CARTESIAN_POINT ( 'NONE',  ( -14.87966828496393035, 178.9354977172588690, 312.8502022180878726 ) ) ;
#7094 = VECTOR ( 'NONE', #10827, 1000.000000000000000 ) ;
#7095 = CIRCLE ( 'NONE', #20666, 83.00000000000002842 ) ;
#7096 = CARTESIAN_POINT ( 'NONE',  ( 19.30212114139425594, 183.2083992702308137, 309.5025285114336384 ) ) ;
#7097 = EDGE_CURVE ( 'NONE', #17948, #13286, #16417, .T. ) ;
#7098 = ADVANCED_FACE ( 'NONE', ( #2829 ), #14929, .F. ) ;
#7099 = CARTESIAN_POINT ( 'NONE',  ( 1.989200010245318895, 70.55908004698136438, -80.50723945831674655 ) ) ;
#7100 = DIRECTION ( 'NONE',  ( 0.000000000000000000, 0.000000000000000000, 1.000000000000000000 ) ) ;
#7101 = EDGE_CURVE ( 'NONE', #6357, #12249, #16040, .T. ) ;
#7102 = ITEM_DEFINED_TRANSFORMATION ( 'NONE', 'NONE', #7341,  #6292 ) ;
#7103 = VECTOR ( 'NONE', #6544, 999.9999999999998863 ) ;
#7104 = CARTESIAN_POINT ( 'NONE',  ( 45.44382132990763523, 164.1908348453399071, 34.04681375850169189 ) ) ;
#7105 = CARTESIAN_POINT ( 'NONE',  ( -162.0000000000000000, 20.00000000000000000, 53.76161406891260697 ) ) ;
#7106 = FACE_OUTER_BOUND ( 'NONE', #13010, .T. ) ;
#7107 = FACE_OUTER_BOUND ( 'NONE', #15836, .T. ) ;
#7108 = VECTOR ( 'NONE', #22664, 1000.000000000000114 ) ;
#7109 = EDGE_CURVE ( 'NONE', #20855, #22352, #2986, .T. ) ;
#7110 = ORIENTED_EDGE ( 'NONE', *, *, #14162, .T. ) ;
#7111 = DIRECTION ( 'NONE',  ( 0.000000000000000000, 0.000000000000000000, 1.000000000000000000 ) ) ;
#7112 = EDGE_CURVE ( 'NONE', #10097, #14863, #20192, .T. ) ;
#7113 = AXIS2_PLACEMENT_3D ( 'NONE', #15512, #15737, #1710 ) ;
#7114 = LINE ( 'NONE', #1613, #6742 ) ;
#7115 = VERTEX_POINT ( 'NONE', #5426 ) ;
#7116 = EDGE_CURVE ( 'NONE', #16665, #9075, #22413, .T. ) ;
#7117 = CARTESIAN_POINT ( 'NONE',  ( -50.13499642684819690, 95.43998192129494385, -44.18671329044839524 ) ) ;
#7118 = ORIENTED_EDGE ( 'NONE', *, *, #21603, .T. ) ;
#7119 = DIRECTION ( 'NONE',  ( -0.01292394549866695240, -0.005513023399711377420, -0.9999012842304693116 ) ) ;
#7120 = CARTESIAN_POINT ( 'NONE',  ( -64.64767546932813502, 126.1473081376430798, 27.67873648630093797 ) ) ;
#7121 = CARTESIAN_POINT ( 'NONE',  ( 65.44129831367571626, 190.1904397277867531, 33.64499135954488196 ) ) ;
#7122 = ADVANCED_FACE ( 'NONE', ( #14538 ), #5890, .F. ) ;
#7123 = ORIENTED_EDGE ( 'NONE', *, *, #12912, .T. ) ;
#7124 = CARTESIAN_POINT ( 'NONE',  ( 84.85051924643074983, 104.5953608974804467, -70.00327014827948346 ) ) ;
#7125 = DIRECTION ( 'NONE',  ( 0.01292394549866738608, 0.005513023399720699824, 0.9999012842304692006 ) ) ;
#7126 = CIRCLE ( 'NONE', #8954, 2.000000000000001332 ) ;
#7127 = B_SPLINE_CURVE_WITH_KNOTS ( 'NONE', 3,
 ( #10000, #1168, #8161, #6446, #20429, #2659 ),
 .UNSPECIFIED., .F., .F.,
 ( 4, 2, 4 ),
 ( 2.380730968275997826E-07, 0.002629065763328383015, 0.005257893453559938333 ),
 .UNSPECIFIED. ) ;
#7128 = CARTESIAN_POINT ( 'NONE',  ( -0.7507300172562465512, 327.2392735797590717, 317.4522180588296578 ) ) ;
#7129 = EDGE_CURVE ( 'NONE', #15161, #15824, #15858, .T. ) ;
#7130 = VERTEX_POINT ( 'NONE', #9220 ) ;
#7131 = EDGE_CURVE ( 'NONE', #13046, #6788, #18764, .T. ) ;
#7132 = AXIS2_PLACEMENT_3D ( 'NONE', #2826, #18234, #7769 ) ;
#7133 = LINE ( 'NONE', #8499, #1445 ) ;
#7134 = CARTESIAN_POINT ( 'NONE',  ( -89.62788137478739259, 89.06476581229102862, 51.83667496493544746 ) ) ;
#7135 = ADVANCED_FACE ( 'NONE', ( #11191 ), #9341, .T. ) ;
#7136 = VERTEX_POINT ( 'NONE', #19663 ) ;
#7137 = VERTEX_POINT ( 'NONE', #3933 ) ;
#7138 = DIRECTION ( 'NONE',  ( 0.01292394549866713108, 0.005513023399725330669, 0.9999012842304692006 ) ) ;
#7139 = CARTESIAN_POINT ( 'NONE',  ( 63.54062731776301121, 169.3797848675314128, -113.3289636997295275 ) ) ;
#7140 =( GEOMETRIC_REPRESENTATION_CONTEXT ( 3 ) GLOBAL_UNCERTAINTY_ASSIGNED_CONTEXT ( ( #3705 ) ) GLOBAL_UNIT_ASSIGNED_CONTEXT ( ( #14811, #6484, #2911 ) ) REPRESENTATION_CONTEXT ( 'NONE', 'WORKASPACE' ) );
#7141 = CARTESIAN_POINT ( 'NONE',  ( 81.73018904534613682, 75.12006735377336497, -5.831974844687870529 ) ) ;
#7142 = DIRECTION ( 'NONE',  ( -0.1296504907605108559, -0.005475273188901296634, -0.9915446392518419971 ) ) ;
#7143 = CARTESIAN_POINT ( 'NONE',  ( -10.78611211158319350, 73.98631237024787310, 133.9739795699840386 ) ) ;
#7144 = ORIENTED_EDGE ( 'NONE', *, *, #12066, .T. ) ;
#7145 = EDGE_CURVE ( 'NONE', #850, #22554, #11069, .T. ) ;
#7146 = CARTESIAN_POINT ( 'NONE',  ( -44.54898248114630377, 168.6907664596094776, 35.18517999664061335 ) ) ;
#7147 = ORIENTED_EDGE ( 'NONE', *, *, #13781, .F. ) ;
#7148 = LINE ( 'NONE', #12437, #4766 ) ;
#7149 = CARTESIAN_POINT ( 'NONE',  ( 92.43457499998882554, 72.00000000000000000, -31.19724316448930423 ) ) ;
#7150 = CARTESIAN_POINT ( 'NONE',  ( -78.41642969337061686, 75.12296263580977040, -3.819052735123477316 ) ) ;
#7151 = CARTESIAN_POINT ( 'NONE',  ( -13.50807349407477886, 164.7335820102402693, 316.8006659633929303 ) ) ;
#7152 = CIRCLE ( 'NONE', #6419, 10.00000000000005684 ) ;
#7153 = DIRECTION ( 'NONE',  ( 0.9934404589540163366, 0.1135548637187051429, -0.01346653032743023309 ) ) ;
#7154 = CARTESIAN_POINT ( 'NONE',  ( -50.95823800333778308, 189.5897628274961164, -73.81394971113282111 ) ) ;
#7155 = FILL_AREA_STYLE ('',( #20929 ) ) ;
#7156 = LINE ( 'NONE', #5409, #4040 ) ;
#7157 = ORIENTED_EDGE ( 'NONE', *, *, #14013, .T. ) ;
#7158 = CARTESIAN_POINT ( 'NONE',  ( -40.15274988607927042, 168.6466622724118452, 27.12781108422596787 ) ) ;
#7159 = ORIENTED_EDGE ( 'NONE', *, *, #15484, .T. ) ;
#7160 = CIRCLE ( 'NONE', #15271, 101.0000000000000000 ) ;
#7161 = ORIENTED_EDGE ( 'NONE', *, *, #7415, .F. ) ;
#7162 = EDGE_LOOP ( 'NONE', ( #2994, #586, #21540, #2709 ) ) ;
#7163 = CARTESIAN_POINT ( 'NONE',  ( 14.29282774033867831, 189.5286527345450338, 308.0677346475730474 ) ) ;
#7164 = EDGE_CURVE ( 'NONE', #17417, #3170, #7764, .T. ) ;
#7166 = ORIENTED_EDGE ( 'NONE', *, *, #3741, .F. ) ;
#7165 = VERTEX_POINT ( 'NONE', #16381 ) ;
#7167 = DIRECTION ( 'NONE',  ( 0.5697992685214862130, 0.5741585497524474002, -0.5879377121248013927 ) ) ;
#7168 = CARTESIAN_POINT ( 'NONE',  ( 3.833582208905060185, 166.6352317792379267, 296.5970240496429255 ) ) ;
#7169 = CARTESIAN_POINT ( 'NONE',  ( -5.871648968083819753, 70.63018678438872655, -88.03282711297042340 ) ) ;
#7170 = DIRECTION ( 'NONE',  ( 1.396592535537253658E-14, 0.000000000000000000, 1.000000000000000000 ) ) ;
#7171 = DIRECTION ( 'NONE',  ( 0.000000000000000000, 1.000000000000000000, 0.000000000000000000 ) ) ;
#7172 = CARTESIAN_POINT ( 'NONE',  ( 38.46706438352715196, 72.00000000000000000, -85.27439087629288395 ) ) ;
#7173 = CARTESIAN_POINT ( 'NONE',  ( 13.02821242091870424, 190.3077089839192695, 320.8514904664418737 ) ) ;
#7174 = AXIS2_PLACEMENT_3D ( 'NONE', #22253, #6543, #7111 ) ;
#7175 = CARTESIAN_POINT ( 'NONE',  ( 80.32251751971472231, 75.20580539967184563, -7.288561962794373628 ) ) ;
#7176 = CARTESIAN_POINT ( 'NONE',  ( 18.21242699821856448, 184.1333206525301875, 308.0386800383396917 ) ) ;
#7177 = CARTESIAN_POINT ( 'NONE',  ( 92.30767208729216122, 77.25770192717985196, 29.02102379856335901 ) ) ;
#7178 = CARTESIAN_POINT ( 'NONE',  ( 92.90824731599337838, 79.04398536104963569, 26.22411128322410789 ) ) ;
#7179 = ORIENTED_EDGE ( 'NONE', *, *, #8950, .T. ) ;
#7180 = DIRECTION ( 'NONE',  ( -7.125109674243555432E-05, 0.9999848031710253382, -0.005512562950850175003 ) ) ;
#7181 = DIRECTION ( 'NONE',  ( 0.009760756503427813965, -0.9999378516499565217, 0.005387065077607405654 ) ) ;
#7182 = ORIENTED_EDGE ( 'NONE', *, *, #9835, .F. ) ;
#7183 = DIRECTION ( 'NONE',  ( -2.025474946048326393E-22, 1.000000000000000000, -1.876735158486679873E-22 ) ) ;
#7184 = VERTEX_POINT ( 'NONE', #16270 ) ;
#7185 = EDGE_CURVE ( 'NONE', #5449, #567, #7271, .T. ) ;
#7186 = EDGE_CURVE ( 'NONE', #6548, #16712, #16936, .T. ) ;
#7187 = AXIS2_PLACEMENT_3D ( 'NONE', #20775, #10451, #1721 ) ;
#7188 = LINE ( 'NONE', #12022, #18027 ) ;
#7189 = SURFACE_SIDE_STYLE ('',( #8664 ) ) ;
#7190 = DIRECTION ( 'NONE',  ( 0.009760756503428008254, -0.9999378516499564107, 0.005387065077611006073 ) ) ;
#7191 = DIRECTION ( 'NONE',  ( -2.025474946048326158E-22, 1.000000000000000000, -1.876735158486678933E-22 ) ) ;
#7192 = CARTESIAN_POINT ( 'NONE',  ( -14.37471740060550118, 109.6998846769365628, 127.3137863664913425 ) ) ;
#7193 = ORIENTED_EDGE ( 'NONE', *, *, #9657, .F. ) ;
#7194 = DIRECTION ( 'NONE',  ( 0.01292394549866733230, 0.005513023399720419666, 0.9999012842304692006 ) ) ;
#7195 = EDGE_LOOP ( 'NONE', ( #3972, #425, #20651, #1549 ) ) ;
#7196 = CARTESIAN_POINT ( 'NONE',  ( 4.039679098813819813, 142.9554882982450010, 294.7945285032504330 ) ) ;
#7197 = DIRECTION ( 'NONE',  ( 0.01292414190464174703, 0.000000000000000000, 0.9999164797902015955 ) ) ;
#7198 = PLANE ( 'NONE',  #21614 ) ;
#7199 =( NAMED_UNIT ( * ) PLANE_ANGLE_UNIT ( ) SI_UNIT ( $, .RADIAN. ) );
#7200 = CARTESIAN_POINT ( 'NONE',  ( -91.52572433156647946, 77.25800443875652945, 31.39760542763772477 ) ) ;
#7201 = CARTESIAN_POINT ( 'NONE',  ( -52.61467855174260677, 126.5883500096206546, 107.5286736637874299 ) ) ;
#7202 = VERTEX_POINT ( 'NONE', #21606 ) ;
#7203 = CARTESIAN_POINT ( 'NONE',  ( -49.64892827247506091, 126.1473081376431367, 27.48487435773119714 ) ) ;
#7204 = PRODUCT_DEFINITION_SHAPE ( 'NONE', 'NONE',  #13264 ) ;
#7205 = CARTESIAN_POINT ( 'NONE',  ( -50.72033869335580647, 114.2302237440943742, 169.5554601261313223 ) ) ;
#7206 = CARTESIAN_POINT ( 'NONE',  ( -5.194761585865951936, 326.6903935298140027, 307.3756461515444585 ) ) ;
#7207 = CARTESIAN_POINT ( 'NONE',  ( -14.85968324574364452, 178.8445255148678541, 318.6896797951268923 ) ) ;
#7209 = ADVANCED_FACE ( 'NONE', ( #16484 ), #6119, .T. ) ;
#7208 =( REPRESENTATION_RELATIONSHIP ('NONE','NONE', #11808, #938 ) REPRESENTATION_RELATIONSHIP_WITH_TRANSFORMATION ( #7660 )SHAPE_REPRESENTATION_RELATIONSHIP( ) );
#7210 = CARTESIAN_POINT ( 'NONE',  ( 20.16435332678968706, 182.3960463823266878, 311.2982132828925614 ) ) ;
#7211 = ORIENTED_EDGE ( 'NONE', *, *, #3608, .F. ) ;
#7212 = EDGE_CURVE ( 'NONE', #16639, #10904, #16931, .T. ) ;
#7213 = DIRECTION ( 'NONE',  ( 0.4768814951561130555, 0.000000000000000000, 0.8789675987075236119 ) ) ;
#7214 = ITEM_DEFINED_TRANSFORMATION ( 'NONE', 'NONE', #15817,  #6292 ) ;
#7215 = CARTESIAN_POINT ( 'NONE',  ( 36.73936676148917968, 94.93197183469658285, 81.60001862646660697 ) ) ;
#7216 = ORIENTED_EDGE ( 'NONE', *, *, #9207, .T. ) ;
#7217 = DIRECTION ( 'NONE',  ( 0.9506032891036972909, -0.3102281881984320644, -0.01057629388542894074 ) ) ;
#7218 = CARTESIAN_POINT ( 'NONE',  ( -53.19734013806819206, 189.4876967392748384, -92.29990616481009624 ) ) ;
#7219 = LINE ( 'NONE', #3655, #8181 ) ;
#7220 = ORIENTED_EDGE ( 'NONE', *, *, #19213, .T. ) ;
#7221 = CARTESIAN_POINT ( 'NONE',  ( 89.71146001588847696, 97.21218566216820989, -63.65427843874460478 ) ) ;
#7222 = CARTESIAN_POINT ( 'NONE',  ( -48.73626655442960498, 109.8645326797279864, -43.54290528015454953 ) ) ;
#7223 = EDGE_CURVE ( 'NONE', #22174, #5625, #8294, .T. ) ;
#7224 = ORIENTED_EDGE ( 'NONE', *, *, #21978, .T. ) ;
#7225 = DIRECTION ( 'NONE',  ( -2.025474946048326158E-22, 1.000000000000000000, -1.876735158486679638E-22 ) ) ;
#7226 = VERTEX_POINT ( 'NONE', #14887 ) ;
#7227 = DIRECTION ( 'NONE',  ( -7.176269450075762180E-19, 1.000000000000000000, -5.550596000020001457E-17 ) ) ;
#7228 = CARTESIAN_POINT ( 'NONE',  ( -88.82263333796718996, 169.9999999999999716, 1.148052203164670715 ) ) ;
#7229 = DIRECTION ( 'NONE',  ( 7.125109674403837105E-05, -0.9999848031710252272, 0.005512562950847867821 ) ) ;
#7230 = ORIENTED_EDGE ( 'NONE', *, *, #9485, .T. ) ;
#7231 = FACE_OUTER_BOUND ( 'NONE', #5510, .T. ) ;
#7232 = CARTESIAN_POINT ( 'NONE',  ( 38.21725127624093687, 94.02752048664899576, 82.48544353620104630 ) ) ;
#7233 = CARTESIAN_POINT ( 'NONE',  ( 21.53177455942607921, 168.7406653857994456, 316.7880417924246785 ) ) ;
#7234 = ORIENTED_EDGE ( 'NONE', *, *, #10354, .T. ) ;
#7235 = ADVANCED_FACE ( 'NONE', ( #7952 ), #12810, .T. ) ;
#7236 = CARTESIAN_POINT ( 'NONE',  ( 90.02055463237803679, 72.00000000000000000, -63.21629334023821656 ) ) ;
#7237 = CARTESIAN_POINT ( 'NONE',  ( -89.91512339040338020, 88.85449468744033652, 52.31052459259786502 ) ) ;
#7238 = EDGE_CURVE ( 'NONE', #15636, #22552, #14420, .T. ) ;
#7239 = ORIENTED_EDGE ( 'NONE', *, *, #4672, .F. ) ;
#7240 = ORIENTED_EDGE ( 'NONE', *, *, #15857, .F. ) ;
#7241 = CARTESIAN_POINT ( 'NONE',  ( -92.43457499998879712, 79.86121811340019860, 31.19724316448926160 ) ) ;
#7242 = CYLINDRICAL_SURFACE ( 'NONE', #457, 8.000000000000000000 ) ;
#7243 = CARTESIAN_POINT ( 'NONE',  ( 81.57020707306168106, 75.12296263580984146, -5.886915439866140076 ) ) ;
#7244 = CIRCLE ( 'NONE', #18264, 2.000000000000001332 ) ;
#7245 = DIRECTION ( 'NONE',  ( -0.01292394549866750231, -0.005513023399722823126, -0.9999012842304692006 ) ) ;
#7246 = ADVANCED_FACE ( 'NONE', ( #2567 ), #18434, .F. ) ;
#7247 = EDGE_LOOP ( 'NONE', ( #16904, #945, #8027, #14041 ) ) ;
#7248 = CARTESIAN_POINT ( 'NONE',  ( 58.87479767622038906, 143.5880916635284166, 105.9939182712553105 ) ) ;
#7249 = VERTEX_POINT ( 'NONE', #21936 ) ;
#7250 = CARTESIAN_POINT ( 'NONE',  ( -55.33804461215960657, 114.2193244133317904, 167.6379947637574617 ) ) ;
#7251 = VECTOR ( 'NONE', #17577, 1000.000000000000227 ) ;
#7252 = DIRECTION ( 'NONE',  ( -7.125109674158749138E-05, 0.9999848031710253382, -0.005512562950850162860 ) ) ;
#7253 = CARTESIAN_POINT ( 'NONE',  ( 0.000000000000000000, 1.999999999999998224, 0.000000000000000000 ) ) ;
#7254 = CARTESIAN_POINT ( 'NONE',  ( -27.37946785251584103, 324.1954850279340121, 317.8131825257059973 ) ) ;
#7255 = ORIENTED_EDGE ( 'NONE', *, *, #6263, .T. ) ;
#7256 = DIRECTION ( 'NONE',  ( 0.000000000000000000, 1.000000000000000000, 0.000000000000000000 ) ) ;
#7257 = EDGE_CURVE ( 'NONE', #15577, #6085, #14024, .T. ) ;
#7258 = ORIENTED_EDGE ( 'NONE', *, *, #9503, .T. ) ;
#7259 = CARTESIAN_POINT ( 'NONE',  ( -39.06289137140529988, 108.3156947416822362, 72.76082051835628306 ) ) ;
#7260 = CARTESIAN_POINT ( 'NONE',  ( 51.99565694909048830, 170.0000000000000284, -0.6720553790413839046 ) ) ;
#7261 = EDGE_LOOP ( 'NONE', ( #6078, #1589, #20520, #20162, #22145 ) ) ;
#7262 = DIRECTION ( 'NONE',  ( 0.000000000000000000, 0.000000000000000000, -1.000000000000000000 ) ) ;
#7263 = EDGE_LOOP ( 'NONE', ( #1440, #22595, #22106, #18815 ) ) ;
#7264 = ORIENTED_EDGE ( 'NONE', *, *, #9282, .F. ) ;
#7265 = CARTESIAN_POINT ( 'NONE',  ( 18.87286229185910358, 185.1068706869312734, 317.5975223423299099 ) ) ;
#7266 = ADVANCED_FACE ( 'NONE', ( #2690 ), #9695, .T. ) ;
#7267 = EDGE_CURVE ( 'NONE', #8873, #13728, #20252, .T. ) ;
#7269 = VERTEX_POINT ( 'NONE', #15222 ) ;
#7268 = ORIENTED_EDGE ( 'NONE', *, *, #10061, .T. ) ;
#7270 = CARTESIAN_POINT ( 'NONE',  ( -44.25520882077128704, 168.2183454221810734, 273.2074843050344271 ) ) ;
#7271 = LINE ( 'NONE', #507, #19496 ) ;
#7272 = DIRECTION ( 'NONE',  ( -0.01292394549866731843, -0.005513023399720594006, -0.9999012842304693116 ) ) ;
#7273 = AXIS2_PLACEMENT_3D ( 'NONE', #20258, #6030, #2812 ) ;
#7274 = DIRECTION ( 'NONE',  ( -1.000000000000000000, 0.000000000000000000, 1.396592535537253658E-14 ) ) ;
#7275 = CARTESIAN_POINT ( 'NONE',  ( -38.40954875669835644, 96.40145467477475449, 84.69856280946498828 ) ) ;
#7276 = SURFACE_STYLE_USAGE ( .BOTH. , #20947 ) ;
#7277 = DIRECTION ( 'NONE',  ( 0.000000000000000000, 0.000000000000000000, 1.000000000000000000 ) ) ;
#7278 = CARTESIAN_POINT ( 'NONE',  ( 17.77085107348584714, 184.5354884815143635, 309.5757466669096516 ) ) ;
#7279 = CARTESIAN_POINT ( 'NONE',  ( 83.75728585524183245, 104.6157580258879136, 71.30770656078364311 ) ) ;
#7280 = CARTESIAN_POINT ( 'NONE',  ( -83.75728585524177561, 104.6157580258879278, -71.30770656078371417 ) ) ;
#7281 = ADVANCED_FACE ( 'NONE', ( #16817 ), #1071, .T. ) ;
#7282 =( LENGTH_UNIT ( ) NAMED_UNIT ( * ) SI_UNIT ( .MILLI., .METRE. ) );
#7283 = CARTESIAN_POINT ( 'NONE',  ( -9.234393433859628075, 186.8255024611774502, 321.3851115294108354 ) ) ;
#7284 = DIRECTION ( 'NONE',  ( 0.01292394549866738782, 0.005513023399720468239, 0.9999012842304692006 ) ) ;
#7285 = EDGE_LOOP ( 'NONE', ( #20641, #18717, #3595, #10265 ) ) ;
#7286 = CARTESIAN_POINT ( 'NONE',  ( -47.87037866543662545, 166.9544368456019470, 276.4614957428762523 ) ) ;
#7287 = AXIS2_PLACEMENT_3D ( 'NONE', #20434, #508, #12799 ) ;
#7288 = ORIENTED_EDGE ( 'NONE', *, *, #9115, .F. ) ;
#7289 = ADVANCED_FACE ( 'NONE', ( #4613 ), #21725, .F. ) ;
#7290 = AXIS2_PLACEMENT_3D ( 'NONE', #22330, #11814, #8336 ) ;
#7291 = ORIENTED_EDGE ( 'NONE', *, *, #18538, .F. ) ;
#7292 = CARTESIAN_POINT ( 'NONE',  ( -39.40254987707573520, 92.58578643762697880, 84.93055112583743949 ) ) ;
#7293 = FILL_AREA_STYLE_COLOUR ( '', #8351 ) ;
#7294 = CARTESIAN_POINT ( 'NONE',  ( 51.99565694909076541, 169.9999999999999716, -0.6720553790413538175 ) ) ;
#7295 = DIRECTION ( 'NONE',  ( 0.01292394549866739996, 0.005513023399720822122, 0.9999012842304692006 ) ) ;
#7296 = CARTESIAN_POINT ( 'NONE',  ( -38.68617183816869698, 163.9153776386440882, 273.1592279730091377 ) ) ;
#7297 = ORIENTED_EDGE ( 'NONE', *, *, #22451, .T. ) ;
#7298 = FACE_OUTER_BOUND ( 'NONE', #6407, .T. ) ;
#7299 = EDGE_LOOP ( 'NONE', ( #255, #11948, #3552, #13856, #1479, #17890 ) ) ;
#7300 = CARTESIAN_POINT ( 'NONE',  ( -64.54563767617682402, 145.1911235850903381, 35.57320806407841474 ) ) ;
#7301 = CIRCLE ( 'NONE', #13199, 109.9999999999999858 ) ;
#7302 = LINE ( 'NONE', #16307, #21768 ) ;
#7303 = CARTESIAN_POINT ( 'NONE',  ( 66.45999312048357410, 69.99999999999998579, -87.65380681892989401 ) ) ;
#7304 = ADVANCED_FACE ( 'NONE', ( #11638, #22176 ), #11295, .T. ) ;
#7305 = CARTESIAN_POINT ( 'NONE',  ( -9.998272952413007175, 187.5299746390215603, 321.1462410811432164 ) ) ;
#7306 = ADVANCED_FACE ( 'NONE', ( #1196 ), #6470, .T. ) ;
#7307 = AXIS2_PLACEMENT_3D ( 'NONE', #20528, #11492, #6319 ) ;
#7308 = CARTESIAN_POINT ( 'NONE',  ( -92.16545979397227484, 77.13735158510579026, 31.20743466190297610 ) ) ;
#7309 = DIRECTION ( 'NONE',  ( 0.01035335185279143318, 0.005513005182356926943, 0.9999312050732649393 ) ) ;
#7310 = ORIENTED_EDGE ( 'NONE', *, *, #649, .T. ) ;
#7311 = CARTESIAN_POINT ( 'NONE',  ( -15.18074383830488294, 179.4905375618960477, 314.9769008739356764 ) ) ;
#7312 = CARTESIAN_POINT ( 'NONE',  ( 40.57355171551004958, 108.0982075334647163, 198.8652726751216733 ) ) ;
#7313 = CARTESIAN_POINT ( 'NONE',  ( -2.669360985930898433, 326.9830943121846190, 308.3414884390720090 ) ) ;
#7314 = CARTESIAN_POINT ( 'NONE',  ( -14.41394558013555560, 181.3065684521603202, 318.0453326090317319 ) ) ;
#7315 = LINE ( 'NONE', #7559, #11002 ) ;
#7316 = VERTEX_POINT ( 'NONE', #13817 ) ;
#7317 = VECTOR ( 'NONE', #9260, 999.9999999999998863 ) ;
#7318 = COLOUR_RGB ( '', 0.31764706, 0.68627451, 0.89019608) ;
#7319 = CARTESIAN_POINT ( 'NONE',  ( 11.85578982808163495, 187.7458312107169434, 305.0703088229346918 ) ) ;
#7320 = ITEM_DEFINED_TRANSFORMATION ( 'NONE', 'NONE', #7729,  #6292 ) ;
#7321 = DIRECTION ( 'NONE',  ( -0.01292394549866738608, -0.005513023399720699824, -0.9999012842304692006 ) ) ;
#7322 = AXIS2_PLACEMENT_3D ( 'NONE', #20986, #19602, #5124 ) ;
#7323 = ORIENTED_EDGE ( 'NONE', *, *, #514, .T. ) ;
#7324 = CARTESIAN_POINT ( 'NONE',  ( -41.84548474893134085, 165.9069838518206836, 244.1862188963381755 ) ) ;
#7325 = DIRECTION ( 'NONE',  ( 0.9999164797902017066, 0.000000000000000000, -0.01292414190463751951 ) ) ;
#7326 = CARTESIAN_POINT ( 'NONE',  ( -49.99582398951010731, 170.0000000000000284, 0.6462070952320568828 ) ) ;
#7327 = ORIENTED_EDGE ( 'NONE', *, *, #21040, .F. ) ;
#7328 = CARTESIAN_POINT ( 'NONE',  ( -65.63430937367742501, 90.62871777570580889, 67.04661370716345914 ) ) ;
#7329 = LINE ( 'NONE', #7794, #19693 ) ;
#7330 = ORIENTED_EDGE ( 'NONE', *, *, #125, .F. ) ;
#7331 = DIRECTION ( 'NONE',  ( -2.025474946048326158E-22, 1.000000000000000000, -1.876735158486679638E-22 ) ) ;
#7332 = VERTEX_POINT ( 'NONE', #5288 ) ;
#7334 = CARTESIAN_POINT ( 'NONE',  ( 45.19575868936945540, 125.3640259171584290, 246.9784031832207631 ) ) ;
#7333 = CARTESIAN_POINT ( 'NONE',  ( 19.42535155401557034, 139.7551263635816952, -44.58871309782323067 ) ) ;
#7335 = DIRECTION ( 'NONE',  ( 0.9232306267972774094, 0.000000000000000000, -0.3842462878721227826 ) ) ;
#7336 = AXIS2_PLACEMENT_3D ( 'NONE', #6935, #183, #10743 ) ;
#7337 = AXIS2_PLACEMENT_3D ( 'NONE', #12243, #21070, #17525 ) ;
#7338 =( REPRESENTATION_RELATIONSHIP ('NONE','NONE', #11808, #21177 ) REPRESENTATION_RELATIONSHIP_WITH_TRANSFORMATION ( #9992 )SHAPE_REPRESENTATION_RELATIONSHIP( ) );
#7339 = VERTEX_POINT ( 'NONE', #17382 ) ;
#7340 = CARTESIAN_POINT ( 'NONE',  ( 36.81267581808855738, 93.81198433751869459, 82.30576130133127322 ) ) ;
#7341 = AXIS2_PLACEMENT_3D ( 'NONE', #16514, #12828, #16305 ) ;
#7342 = CARTESIAN_POINT ( 'NONE',  ( 20.04619608162330024, 168.5799960362341210, 319.0729041454727621 ) ) ;
#7343 = ORIENTED_EDGE ( 'NONE', *, *, #3028, .F. ) ;
#7344 = DIRECTION ( 'NONE',  ( -0.01292394549866637994, -0.005513023399719273882, -0.9999012842304692006 ) ) ;
#7345 = CARTESIAN_POINT ( 'NONE',  ( -89.67433851549336055, 89.04342406756380512, 51.90552969022834873 ) ) ;
#7346 = AXIS2_PLACEMENT_3D ( 'NONE', #22407, #9081, #14062 ) ;
#7347 = ORIENTED_EDGE ( 'NONE', *, *, #4727, .T. ) ;
#7348 = CIRCLE ( 'NONE', #13957, 2.499999999999988010 ) ;
#7349 = ORIENTED_EDGE ( 'NONE', *, *, #20498, .F. ) ;
#7350 = LINE ( 'NONE', #21362, #16617 ) ;
#7351 = AXIS2_PLACEMENT_3D ( 'NONE', #6038, #2592, #6264 ) ;
#7352 =( BOUNDED_CURVE ( )  B_SPLINE_CURVE ( 3, ( #10840, #8738, #17866, #19211 ),
 .UNSPECIFIED., .F., .T. ) 
 B_SPLINE_CURVE_WITH_KNOTS ( ( 4, 4 ),
 ( 5.799006443144740786, 5.860216683781459324 ),
 .UNSPECIFIED. ) 
 CURVE ( )  GEOMETRIC_REPRESENTATION_ITEM ( )  RATIONAL_B_SPLINE_CURVE ( ( 1.000000000000000000, 0.9996877999070342691, 0.9996877999070342691, 1.000000000000000000 ) ) 
 REPRESENTATION_ITEM ( '' )  );
#7353 = DIRECTION ( 'NONE',  ( 0.01220060921879500236, -0.3298969072164960603, 0.9439381207174974975 ) ) ;
#7354 = LINE ( 'NONE', #20882, #7468 ) ;
#7355 = DIRECTION ( 'NONE',  ( -0.000000000000000000, -1.000000000000000000, 0.000000000000000000 ) ) ;
#7356 = EDGE_CURVE ( 'NONE', #12, #7696, #20481, .T. ) ;
#7357 = DIRECTION ( 'NONE',  ( 7.125109674160325297E-05, -0.9999848031710252272, 0.005512562950849327591 ) ) ;
#7358 = ORIENTED_EDGE ( 'NONE', *, *, #4970, .T. ) ;
#7359 = DIRECTION ( 'NONE',  ( -0.9934404589540162256, -0.1135548637187055315, 0.01346653032743023309 ) ) ;
#7360 = CIRCLE ( 'NONE', #1861, 7.499999999999991118 ) ;
#7361 = EDGE_LOOP ( 'NONE', ( #11522, #11222, #7230, #2102, #14893, #21988 ) ) ;
#7362 = CARTESIAN_POINT ( 'NONE',  ( 0.000000000000000000, 20.00000000000000000, 124.0000000000000000 ) ) ;
#7363 = LINE ( 'NONE', #12678, #16678 ) ;
#7364 = CARTESIAN_POINT ( 'NONE',  ( -78.28836335706589011, 75.12327740397419973, 5.852126302717420181 ) ) ;
#7365 = CARTESIAN_POINT ( 'NONE',  ( -12.91084759039031127, 164.8071687891488750, 318.1111553772653338 ) ) ;
#7366 = EDGE_CURVE ( 'NONE', #12349, #13772, #19861, .T. ) ;
#7367 = CARTESIAN_POINT ( 'NONE',  ( -1.163172771417702700, 81.99999999999998579, -89.99248318111824574 ) ) ;
#7368 = VERTEX_POINT ( 'NONE', #22392 ) ;
#7369 = FACE_OUTER_BOUND ( 'NONE', #15788, .T. ) ;
#7370 = CARTESIAN_POINT ( 'NONE',  ( 14.14224087380716455, 105.6999953372425409, 126.9762993157022777 ) ) ;
#7371 = CYLINDRICAL_SURFACE ( 'NONE', #14358, 10.00000000000001599 ) ;
#7372 = ORIENTED_EDGE ( 'NONE', *, *, #19041, .F. ) ;
#7373 = CIRCLE ( 'NONE', #20199, 1.999999999999998224 ) ;
#7374 = DIRECTION ( 'NONE',  ( 0.01292394549866741384, 0.005513023399720270480, 0.9999012842304693116 ) ) ;
#7375 = ORIENTED_EDGE ( 'NONE', *, *, #17938, .F. ) ;
#7376 = AXIS2_PLACEMENT_3D ( 'NONE', #22067, #4390, #20248 ) ;
#7377 = VERTEX_POINT ( 'NONE', #20571 ) ;
#7378 = DIRECTION ( 'NONE',  ( -5.440186201345738641E-18, -1.000000000000000000, -1.334940939666364181E-17 ) ) ;
#7379 = EDGE_CURVE ( 'NONE', #2060, #14939, #10581, .T. ) ;
#7380 = CARTESIAN_POINT ( 'NONE',  ( 17.75217047904729384, 186.5091196593482721, 318.8417065694452504 ) ) ;
#7381 = CIRCLE ( 'NONE', #10686, 3.047499999999988329 ) ;
#7382 = ORIENTED_EDGE ( 'NONE', *, *, #2951, .F. ) ;
#7383 = EDGE_CURVE ( 'NONE', #14816, #1810, #16258, .T. ) ;
#7384 = DIRECTION ( 'NONE',  ( 0.01292394549866695240, 0.005513023399725255208, 0.9999012842304693116 ) ) ;
#7385 = DIRECTION ( 'NONE',  ( -0.01292394549866731843, -0.005513023399720594006, -0.9999012842304693116 ) ) ;
#7386 = LINE ( 'NONE', #7512, #20496 ) ;
#7387 = B_SPLINE_CURVE_WITH_KNOTS ( 'NONE', 3,
 ( #15963, #2035, #10985, #7084, #7547, #21093, #21202, #86, #10878, #3523 ),
 .UNSPECIFIED., .F., .F.,
 ( 4, 2, 2, 2, 4 ),
 ( 5.721958498152796815E-17, 0.0004376694309007161097, 0.0008753388618013749735, 0.001313008292702033892, 0.001750677723602692701 ),
 .UNSPECIFIED. ) ;
#7388 = CARTESIAN_POINT ( 'NONE',  ( -91.14933227754934819, 79.20679280668173305, -26.78161688013030428 ) ) ;
#7389 = CIRCLE ( 'NONE', #17309, 8.000000000000014211 ) ;
#7390 = DIRECTION ( 'NONE',  ( -0.9909299940865186063, 0.1338359446631179339, 0.01207007604875938098 ) ) ;
#7391 =( GEOMETRIC_REPRESENTATION_CONTEXT ( 3 ) GLOBAL_UNCERTAINTY_ASSIGNED_CONTEXT ( ( #5078 ) ) GLOBAL_UNIT_ASSIGNED_CONTEXT ( ( #10154, #18759, #15454 ) ) REPRESENTATION_CONTEXT ( 'NONE', 'WORKASPACE' ) );
#7392 = DIRECTION ( 'NONE',  ( -0.000000000000000000, -1.000000000000000000, 0.000000000000000000 ) ) ;
#7393 = DIRECTION ( 'NONE',  ( 0.000000000000000000, 1.000000000000000000, -0.000000000000000000 ) ) ;
#7394 = VECTOR ( 'NONE', #18935, 1000.000000000000114 ) ;
#7395 = CARTESIAN_POINT ( 'NONE',  ( 19.46619799173079812, 184.1572589165842260, 312.1803994612432120 ) ) ;
#7396 = CARTESIAN_POINT ( 'NONE',  ( 89.70716773419727019, 79.66972452536271021, 28.26220109401201341 ) ) ;
#7397 = ADVANCED_FACE ( 'NONE', ( #1637 ), #20912, .T. ) ;
#7398 = B_SPLINE_CURVE_WITH_KNOTS ( 'NONE', 3,
 ( #5962, #7683, #1964, #7340, #19521, #3792, #7232, #8953 ),
 .UNSPECIFIED., .F., .F.,
 ( 4, 2, 2, 4 ),
 ( 0.000000000000000000, 0.0007138554872576933965, 0.001427710974515386793, 0.002855421949030781392 ),
 .UNSPECIFIED. ) ;
#7399 = ADVANCED_FACE ( 'NONE', ( #18858 ), #3466, .F. ) ;
#7400 = CARTESIAN_POINT ( 'NONE',  ( 89.22440607450265304, 80.22990097357060790, 29.93634654116225846 ) ) ;
#7401 = VERTEX_POINT ( 'NONE', #4829 ) ;
#7402 = CIRCLE ( 'NONE', #16602, 10.71774939102741264 ) ;
#7403 = DIRECTION ( 'NONE',  ( -0.01292394549866632963, -0.005513023399716958026, -0.9999012842304692006 ) ) ;
#7404 = EDGE_CURVE ( 'NONE', #7269, #4506, #20800, .T. ) ;
#7405 = DIRECTION ( 'NONE',  ( -0.9999164797902017066, -2.001050586450178931E-22, 0.01292414190464131508 ) ) ;
#7406 = DIRECTION ( 'NONE',  ( -0.009188991635466043154, 0.7031977391749434370, -0.7109349492407667226 ) ) ;
#7407 = VERTEX_POINT ( 'NONE', #5172 ) ;
#7408 = B_SPLINE_CURVE_WITH_KNOTS ( 'NONE', 3,
 ( #21146, #10583, #142, #17261, #19311, #7243, #7141, #7025, #6904, #13924, #20916, #1530, #5174, #8622, #8725, #1857, #8513, #21037, #10484, #5392, #19081, #12215, #15665, #22608, #19199, #3470, #12431, #18965, #19, #1747, #19419, #15554, #3681, #15778, #14053, #10702, #8968, #17731, #1977, #22503 ),
 .UNSPECIFIED., .F., .F.,
 ( 4, 2, 2, 2, 2, 2, 2, 2, 2, 2, 2, 2, 2, 2, 2, 2, 2, 2, 2, 4 ),
 ( 0.000000000000000000, 0.0009967370484891076212, 0.001495105572733641157, 0.001993474096978174476, 0.002990211145467242416, 0.003986948193956310789, 0.004983685242445377861, 0.005980422290934445800, 0.006977159339423513740, 0.007973896387912581679, 0.008970633436401647884, 0.009967370484890715823, 0.01046573900913524979, 0.01096410753337978376, 0.01196084458186887599, 0.01295758163035796821, 0.01345595015460251606, 0.01395431867884706217, 0.01495105572733619256, 0.01594779277582532295 ),
 .UNSPECIFIED. ) ;
#7410 = PLANE ( 'NONE',  #12421 ) ;
#7409 = AXIS2_PLACEMENT_3D ( 'NONE', #13289, #16509, #886 ) ;
#7411 = ORIENTED_EDGE ( 'NONE', *, *, #388, .T. ) ;
#7412 = TOROIDAL_SURFACE ( 'NONE', #15148, 124.0000000000000000, 2.000000000000000000 ) ;
#7413 = AXIS2_PLACEMENT_3D ( 'NONE', #1701, #18813, #11694 ) ;
#7414 = CARTESIAN_POINT ( 'NONE',  ( -44.97237925423871019, 166.7992958956050416, 308.9781073544560854 ) ) ;
#7415 = EDGE_CURVE ( 'NONE', #14939, #16331, #3221, .T. ) ;
#7416 = AXIS2_PLACEMENT_3D ( 'NONE', #15437, #19197, #17492 ) ;
#7417 = CARTESIAN_POINT ( 'NONE',  ( -64.14341903774379716, 91.03664218477042880, 66.69210539709879981 ) ) ;
#7418 = FACE_OUTER_BOUND ( 'NONE', #11048, .T. ) ;
#7419 = DIRECTION ( 'NONE',  ( 0.9999164797902015955, 0.000000000000000000, -0.01292414190464144692 ) ) ;
#7420 = CARTESIAN_POINT ( 'NONE',  ( 14.13996083871143306, 137.6995090387153482, 126.7998973012750810 ) ) ;
#7421 = ORIENTED_EDGE ( 'NONE', *, *, #19002, .T. ) ;
#7422 = DIRECTION ( 'NONE',  ( 0.01292394549866738782, 0.005513023399720468239, 0.9999012842304692006 ) ) ;
#7423 = VERTEX_POINT ( 'NONE', #22605 ) ;
#7424 = VERTEX_POINT ( 'NONE', #15661 ) ;
#7425 = VECTOR ( 'NONE', #17171, 1000.000000000000114 ) ;
#7426 = CARTESIAN_POINT ( 'NONE',  ( 163.9999999999992610, 20.00000000000000000, 53.76161406891480965 ) ) ;
#7427 = ADVANCED_FACE ( 'NONE', ( #8722 ), #9982, .F. ) ;
#7428 = CARTESIAN_POINT ( 'NONE',  ( 68.01573619543682980, 70.58429683895612072, -86.45204278734176739 ) ) ;
#7429 = CARTESIAN_POINT ( 'NONE',  ( -9.904114228265054720, 184.8598382391072619, 321.2234604397826843 ) ) ;
#7430 = CARTESIAN_POINT ( 'NONE',  ( -92.02635692360499320, 79.83422912033660168, 31.21470397902808358 ) ) ;
#7431 = DIRECTION ( 'NONE',  ( 0.01035335185279153900, 0.005513005182355262476, 0.9999312050732647172 ) ) ;
#7432 = VERTEX_POINT ( 'NONE', #21036 ) ;
#7433 = DIRECTION ( 'NONE',  ( -1.000000000000000000, 0.000000000000000000, -1.387778780781444413E-14 ) ) ;
#7434 = VERTEX_POINT ( 'NONE', #12329 ) ;
#7435 = DIRECTION ( 'NONE',  ( 0.000000000000000000, 0.000000000000000000, -1.000000000000000000 ) ) ;
#7436 = AXIS2_PLACEMENT_3D ( 'NONE', #9037, #12639, #7565 ) ;
#7437 = CARTESIAN_POINT ( 'NONE',  ( -14.91916526940173782, 178.8222960241703845, 316.3378698738634398 ) ) ;
#7438 = VERTEX_POINT ( 'NONE', #10245 ) ;
#7439 = ORIENTED_EDGE ( 'NONE', *, *, #17369, .F. ) ;
#7440 = FACE_BOUND ( 'NONE', #1635, .T. ) ;
#7441 = VERTEX_POINT ( 'NONE', #10140 ) ;
#7442 = VECTOR ( 'NONE', #21878, 1000.000000000000000 ) ;
#7443 = AXIS2_PLACEMENT_3D ( 'NONE', #4890, #16062, #2028 ) ;
#7444 = CARTESIAN_POINT ( 'NONE',  ( 11.87689086465382715, 187.8426365274682439, 305.6410650122883794 ) ) ;
#7445 = EDGE_CURVE ( 'NONE', #10110, #10707, #17145, .T. ) ;
#7446 = ITEM_DEFINED_TRANSFORMATION ( 'NONE', 'NONE', #6253,  #6292 ) ;
#7447 = EDGE_CURVE ( 'NONE', #9718, #21686, #12087, .T. ) ;
#7448 = ORIENTED_EDGE ( 'NONE', *, *, #10894, .T. ) ;
#7449 = LINE ( 'NONE', #21451, #21721 ) ;
#7450 = ADVANCED_BREP_SHAPE_REPRESENTATION ( '', ( #9845, #6292 ), #7758 ) ;
#7451 = DIRECTION ( 'NONE',  ( -0.7562662552911951774, 0.5735764363510490460, 0.3147561322209052603 ) ) ;
#7452 = CIRCLE ( 'NONE', #130, 4.200000000000005507 ) ;
#7453 = ORIENTED_EDGE ( 'NONE', *, *, #9222, .T. ) ;
#7454 = DIRECTION ( 'NONE',  ( 0.003413786507415475339, -0.9644842718275420390, 0.2641182225045781706 ) ) ;
#7455 = CARTESIAN_POINT ( 'NONE',  ( -49.51659781732259802, 95.13602058458445754, -43.68511678575673329 ) ) ;
#7456 = EDGE_LOOP ( 'NONE', ( #12336, #5508, #2027, #9177 ) ) ;
#7457 = ORIENTED_EDGE ( 'NONE', *, *, #1718, .F. ) ;
#7458 = CARTESIAN_POINT ( 'NONE',  ( -2.616420304248261886, 190.0885906883363816, 274.8459139047729423 ) ) ;
#7460 = CARTESIAN_POINT ( 'NONE',  ( -51.99565694909051672, 170.0000000000000284, 0.6720553790413400508 ) ) ;
#7459 = PLANE ( 'NONE',  #4553 ) ;
#7461 = CARTESIAN_POINT ( 'NONE',  ( -40.92438434402757963, 95.47920540267311651, -42.72851707616362660 ) ) ;
#7462 = LINE ( 'NONE', #19842, #8860 ) ;
#7463 = CIRCLE ( 'NONE', #11127, 2.000000000000007550 ) ;
#7464 = VERTEX_POINT ( 'NONE', #13921 ) ;
#7465 = CARTESIAN_POINT ( 'NONE',  ( 15.73089101666271361, 145.5050201865991539, 277.3435683618253620 ) ) ;
#7466 = CARTESIAN_POINT ( 'NONE',  ( -162.0000000000000000, 0.000000000000000000, 10.00000000000001776 ) ) ;
#7467 = ORIENTED_EDGE ( 'NONE', *, *, #15841, .T. ) ;
#7468 = VECTOR ( 'NONE', #10668, 999.9999999999998863 ) ;
#7469 = DIRECTION ( 'NONE',  ( -0.000000000000000000, -1.000000000000000000, -0.000000000000000000 ) ) ;
#7470 = CARTESIAN_POINT ( 'NONE',  ( -88.17056478026623267, 88.79561276468949416, 52.25202260040794755 ) ) ;
#7471 = EDGE_CURVE ( 'NONE', #22322, #20464, #21693, .T. ) ;
#7472 = PRODUCT_CONTEXT ( 'NONE', #3389, 'mechanical' ) ;
#7473 = VECTOR ( 'NONE', #15809, 1000.000000000000114 ) ;
#7475 = VERTEX_POINT ( 'NONE', #15775 ) ;
#7474 = ORIENTED_EDGE ( 'NONE', *, *, #240, .F. ) ;
#7476 = CONICAL_SURFACE ( 'NONE', #6747, 117.0000000000000000, 0.3316125578789227979 ) ;
#7477 = ORIENTED_EDGE ( 'NONE', *, *, #772, .T. ) ;
#7478 = PLANE ( 'NONE',  #2999 ) ;
#7479 = CARTESIAN_POINT ( 'NONE',  ( 68.30941429790007646, 191.4143309225247549, 255.6230893828509352 ) ) ;
#7480 = ORIENTED_EDGE ( 'NONE', *, *, #510, .F. ) ;
#7481 = PLANE ( 'NONE',  #18905 ) ;
#7482 = CARTESIAN_POINT ( 'NONE',  ( -10.85624112972181621, 113.6998737626107641, 127.2553023597115214 ) ) ;
#7483 = CARTESIAN_POINT ( 'NONE',  ( -91.10494378670937010, 97.90071567704920596, -61.64404307423189522 ) ) ;
#7484 = VERTEX_POINT ( 'NONE', #16 ) ;
#7485 = CARTESIAN_POINT ( 'NONE',  ( -14.55838832409743056, 177.6144908738019694, 111.6381734428085224 ) ) ;
#7486 = EDGE_LOOP ( 'NONE', ( #4977, #14173, #10435, #14164 ) ) ;
#7487 = CARTESIAN_POINT ( 'NONE',  ( -57.55221044392004615, 114.6951352185433421, 172.9675203174990088 ) ) ;
#7488 = DIRECTION ( 'NONE',  ( 0.9999164797902015955, 8.772500386246550856E-18, -0.01292414190464154927 ) ) ;
#7489 = CIRCLE ( 'NONE', #8569, 4.199999999999997513 ) ;
#7490 = DIRECTION ( 'NONE',  ( 0.000000000000000000, 0.000000000000000000, -1.000000000000000000 ) ) ;
#7491 = FACE_OUTER_BOUND ( 'NONE', #4544, .T. ) ;
#7492 = PRODUCT_DEFINITION ( 'UNKNOWN', '', #4767, #15494 ) ;
#7493 = DIRECTION ( 'NONE',  ( -5.440186201345738641E-18, -1.000000000000000000, -1.334940939666364181E-17 ) ) ;
#7494 = CARTESIAN_POINT ( 'NONE',  ( -40.58168163415708563, 127.0293918815982011, 187.3786108412739395 ) ) ;
#7495 = CARTESIAN_POINT ( 'NONE',  ( -46.79626760996151802, 121.2962013336460814, 248.1898487183183875 ) ) ;
#7496 = AXIS2_PLACEMENT_3D ( 'NONE', #17323, #19257, #15196 ) ;
#7497 = FACE_OUTER_BOUND ( 'NONE', #3986, .T. ) ;
#7498 = EDGE_LOOP ( 'NONE', ( #5829, #18749, #2831, #22416, #4821 ) ) ;
#7499 = AXIS2_PLACEMENT_3D ( 'NONE', #21112, #19383, #3649 ) ;
#7500 = DIRECTION ( 'NONE',  ( -0.7912924530843117310, 0.6113994113550570431, 0.006856638134102506846 ) ) ;
#7501 = B_SPLINE_CURVE_WITH_KNOTS ( 'NONE', 3,
 ( #14745, #943, #7590, #9191, #482, #14625, #7483, #14516, #21477, #21578, #21698, #3412 ),
 .UNSPECIFIED., .F., .F.,
 ( 4, 2, 2, 2, 2, 4 ),
 ( 0.000000000000000000, 0.0007983727002588498134, 0.001596745400517699627, 0.003193490801035416167, 0.004790236201553133358, 0.006386981602070849681 ),
 .UNSPECIFIED. ) ;
#7502 = CARTESIAN_POINT ( 'NONE',  ( 66.06691928577360784, 94.02752048664899576, 82.12548041065294058 ) ) ;
#7503 = ORIENTED_EDGE ( 'NONE', *, *, #6131, .T. ) ;
#7504 = ORIENTED_EDGE ( 'NONE', *, *, #5709, .T. ) ;
#7505 = ORIENTED_EDGE ( 'NONE', *, *, #17396, .F. ) ;
#7506 = CARTESIAN_POINT ( 'NONE',  ( -105.0923722050658426, 70.19488773545516835, 32.49013605942701588 ) ) ;
#7507 = CARTESIAN_POINT ( 'NONE',  ( 19.94236535209076422, 183.5044621163393685, 314.4921078799457064 ) ) ;
#7508 =( BOUNDED_CURVE ( )  B_SPLINE_CURVE ( 3, ( #19796, #4071, #885, #4188 ),
 .UNSPECIFIED., .F., .T. ) 
 B_SPLINE_CURVE_WITH_KNOTS ( ( 4, 4 ),
 ( 0.4472747960204460083, 0.4841788640348455020 ),
 .UNSPECIFIED. ) 
 CURVE ( )  GEOMETRIC_REPRESENTATION_ITEM ( )  RATIONAL_B_SPLINE_CURVE ( ( 1.000000000000000000, 0.9998865107004337727, 0.9998865107004337727, 1.000000000000000000 ) ) 
 REPRESENTATION_ITEM ( '' )  );
#7509 = ADVANCED_FACE ( 'NONE', ( #5513 ), #4826, .T. ) ;
#7510 = ORIENTED_EDGE ( 'NONE', *, *, #6669, .F. ) ;
#7511 = DIRECTION ( 'NONE',  ( -0.01292414190464131335, -1.902755938799530239E-22, -0.9999164797902015955 ) ) ;
#7512 = CARTESIAN_POINT ( 'NONE',  ( 8.633533809377713197, 190.8419313418282854, 256.3975693155348381 ) ) ;
#7513 = AXIS2_PLACEMENT_3D ( 'NONE', #14795, #15006, #20262 ) ;
#7514 = CARTESIAN_POINT ( 'NONE',  ( 5.474031775163560098, 70.55988472974013348, -97.46771346163548344 ) ) ;
#7515 = FACE_OUTER_BOUND ( 'NONE', #21381, .T. ) ;
#7516 = CARTESIAN_POINT ( 'NONE',  ( -22.49358496127553053, 324.7653478115767030, 320.5678661935268678 ) ) ;
#7517 = CARTESIAN_POINT ( 'NONE',  ( 12.86429881287754284, 189.0102787272791716, 276.1886381430309143 ) ) ;
#7518 = CARTESIAN_POINT ( 'NONE',  ( 19.63801391595304935, 182.9631121645107044, 312.1752918911519714 ) ) ;
#7519 = CARTESIAN_POINT ( 'NONE',  ( 91.69446324238793977, 77.56197482480291683, 29.51646066538733493 ) ) ;
#7520 = EDGE_CURVE ( 'NONE', #21699, #4461, #5391, .T. ) ;
#7521 = CARTESIAN_POINT ( 'NONE',  ( -164.0000000000000000, 18.00000000000000355, -7.999999999999979572 ) ) ;
#7522 =( NAMED_UNIT ( * ) SI_UNIT ( $, .STERADIAN. ) SOLID_ANGLE_UNIT ( ) );
#7523 = CARTESIAN_POINT ( 'NONE',  ( 91.51031840793916672, 96.48503848149371720, 61.03988419336475602 ) ) ;
#7524 = CIRCLE ( 'NONE', #20351, 7.499999999999991118 ) ;
#7525 = EDGE_CURVE ( 'NONE', #15481, #12773, #15138, .T. ) ;
#7526 = CARTESIAN_POINT ( 'NONE',  ( -9.804288294571927409, 187.7022783261437837, 321.1616740932373091 ) ) ;
#7527 = DIRECTION ( 'NONE',  ( -5.440186201345738641E-18, -1.000000000000000000, -1.334940939666364181E-17 ) ) ;
#7528 = ORIENTED_EDGE ( 'NONE', *, *, #14135, .F. ) ;
#7529 = DIRECTION ( 'NONE',  ( 0.9999164797902015955, 2.001050586450180341E-22, -0.01292414190464038874 ) ) ;
#7530 = VERTEX_POINT ( 'NONE', #7139 ) ;
#7531 = CYLINDRICAL_SURFACE ( 'NONE', #20705, 2.000000000000003997 ) ;
#7532 = EDGE_CURVE ( 'NONE', #6360, #21645, #1913, .T. ) ;
#7533 = CARTESIAN_POINT ( 'NONE',  ( -37.51181209962059881, 93.56461422141713058, 83.92720337889271320 ) ) ;
#7534 = EDGE_CURVE ( 'NONE', #1183, #13714, #3002, .T. ) ;
#7535 = CARTESIAN_POINT ( 'NONE',  ( 20.96603472858062034, 99.74539563421258492, 74.61103786048235520 ) ) ;
#7536 = CARTESIAN_POINT ( 'NONE',  ( 146.4999999999998579, 0.000000000000000000, -10.00000000000202682 ) ) ;
#7537 = CARTESIAN_POINT ( 'NONE',  ( 163.9999999999998863, 1.999999999999998224, 8.000000000002229328 ) ) ;
#7538 =( GEOMETRIC_REPRESENTATION_CONTEXT ( 3 ) GLOBAL_UNCERTAINTY_ASSIGNED_CONTEXT ( ( #16680 ) ) GLOBAL_UNIT_ASSIGNED_CONTEXT ( ( #5156, #1839, #3332 ) ) REPRESENTATION_CONTEXT ( 'NONE', 'WORKASPACE' ) );
#7539 = DIRECTION ( 'NONE',  ( -0.9999164797902017066, -2.001050586450178931E-22, 0.01292414190464131508 ) ) ;
#7540 = CARTESIAN_POINT ( 'NONE',  ( -9.829296516163982034, 187.6860858752735908, 321.1599732488574546 ) ) ;
#7541 = CARTESIAN_POINT ( 'NONE',  ( 163.1715728752537018, -2.184664232470859687E-16, 8.828427124748404964 ) ) ;
#7542 = VERTEX_POINT ( 'NONE', #141 ) ;
#7543 = CARTESIAN_POINT ( 'NONE',  ( -47.66114072508762689, 168.8134312302532862, 57.47692565324432934 ) ) ;
#7544 = DIRECTION ( 'NONE',  ( 7.855523120248383534E-07, -0.01102495835474487547, -0.9999392232994258611 ) ) ;
#7545 = DIRECTION ( 'NONE',  ( -0.01292394549866741557, -0.005513023399720270480, -0.9999012842304693116 ) ) ;
#7546 = EDGE_CURVE ( 'NONE', #3194, #18220, #478, .T. ) ;
#7547 = CARTESIAN_POINT ( 'NONE',  ( 71.18985671402978710, 92.11167198312701032, 83.85708946072357151 ) ) ;
#7548 = CARTESIAN_POINT ( 'NONE',  ( -9.773826842965361195, 187.7219482422972590, 321.1637457204829502 ) ) ;
#7549 = CARTESIAN_POINT ( 'NONE',  ( -91.77247882320317274, 77.19421037201389879, 31.29629296514997705 ) ) ;
#7550 = DIRECTION ( 'NONE',  ( -0.009138748381789078140, 0.7071067811865487940, -0.7070477234798315802 ) ) ;
#7551 = ORIENTED_EDGE ( 'NONE', *, *, #14314, .F. ) ;
#7552 = CARTESIAN_POINT ( 'NONE',  ( -14.41756379550612799, 181.3026149279955632, 318.0496679571880918 ) ) ;
#7553 = ADVANCED_FACE ( 'NONE', ( #16013 ), #7242, .F. ) ;
#7554 = DIRECTION ( 'NONE',  ( -7.125109674118361251E-05, 0.9999848031710253382, -0.005512562950849477644 ) ) ;
#7555 = CARTESIAN_POINT ( 'NONE',  ( -15.14343016516442120, 179.5770291343474696, 315.4979406396071226 ) ) ;
#7556 = ORIENTED_EDGE ( 'NONE', *, *, #5824, .T. ) ;
#7557 = AXIS2_PLACEMENT_3D ( 'NONE', #15070, #3097, #4353 ) ;
#7558 = ORIENTED_EDGE ( 'NONE', *, *, #19238, .T. ) ;
#7559 = CARTESIAN_POINT ( 'NONE',  ( -64.54884397553028919, 190.1904397277864973, 35.32514273129018534 ) ) ;
#7560 = ORIENTED_EDGE ( 'NONE', *, *, #15429, .T. ) ;
#7561 = DIRECTION ( 'NONE',  ( -0.01292394549866695240, -0.005513023399725255208, -0.9999012842304693116 ) ) ;
#7562 = EDGE_CURVE ( 'NONE', #9818, #19234, #13318, .T. ) ;
#7563 = ORIENTED_EDGE ( 'NONE', *, *, #21170, .T. ) ;
#7564 = CARTESIAN_POINT ( 'NONE',  ( -154.0000000000000000, 18.00000000000000355, 53.76161406891259986 ) ) ;
#7565 = DIRECTION ( 'NONE',  ( -6.938893903907222067E-15, -1.000000000000000000, 0.000000000000000000 ) ) ;
#7566 = ORIENTED_EDGE ( 'NONE', *, *, #20473, .F. ) ;
#7567 = DIRECTION ( 'NONE',  ( 0.1296504907605101897, 0.005475273188901850878, 0.9915446392518421082 ) ) ;
#7568 = ORIENTED_EDGE ( 'NONE', *, *, #7964, .F. ) ;
#7569 = LINE ( 'NONE', #456, #21977 ) ;
#7570 = ORIENTED_EDGE ( 'NONE', *, *, #2780, .T. ) ;
#7571 = CARTESIAN_POINT ( 'NONE',  ( -64.14035809025482138, 91.69347899441576999, 66.92892513032199986 ) ) ;
#7572 = VERTEX_POINT ( 'NONE', #12769 ) ;
#7573 = CARTESIAN_POINT ( 'NONE',  ( 12.91228556302839792, 190.0204481364067988, 320.8669068103490076 ) ) ;
#7574 = CARTESIAN_POINT ( 'NONE',  ( -41.27422076403988171, 95.25460172568500639, -43.11209833513134981 ) ) ;
#7575 = CARTESIAN_POINT ( 'NONE',  ( 25.08966747280857845, 89.38128957862194568, 78.14996769037233548 ) ) ;
#7576 = ADVANCED_FACE ( 'NONE', ( #8966 ), #12188, .T. ) ;
#7577 = CARTESIAN_POINT ( 'NONE',  ( 17.62523603308973463, 146.7439693644061265, 277.9400347667066171 ) ) ;
#7578 = CARTESIAN_POINT ( 'NONE',  ( -164.0000000000000284, 0.8284271247461896248, 8.000000000000019540 ) ) ;
#7579 = ORIENTED_EDGE ( 'NONE', *, *, #22380, .T. ) ;
#7580 = CARTESIAN_POINT ( 'NONE',  ( 42.26887782499613877, 106.8826913590880139, 70.46105996506696556 ) ) ;
#7581 = CARTESIAN_POINT ( 'NONE',  ( -89.08844981478657132, 89.10459688240003118, 51.16498045765563063 ) ) ;
#7582 = EDGE_CURVE ( 'NONE', #17225, #11720, #12669, .T. ) ;
#7583 = ORIENTED_EDGE ( 'NONE', *, *, #12048, .F. ) ;
#7584 = CARTESIAN_POINT ( 'NONE',  ( 0.000000000000000000, 0.000000000000000000, 0.000000000000000000 ) ) ;
#7585 = DIRECTION ( 'NONE',  ( 0.009088227368120101179, 0.7109943316365099353, 0.7031390079522383818 ) ) ;
#7586 = ORIENTED_EDGE ( 'NONE', *, *, #6929, .F. ) ;
#7587 = DIRECTION ( 'NONE',  ( 5.440186201345785633E-18, 1.000000000000000000, 1.334940939666367878E-17 ) ) ;
#7588 = CARTESIAN_POINT ( 'NONE',  ( -8.562029719258356764, 342.2165115496170529, 328.2923693891043513 ) ) ;
#7589 = CARTESIAN_POINT ( 'NONE',  ( -106.0703656581358416, 70.66226986180335246, -29.13909619158257769 ) ) ;
#7590 = CARTESIAN_POINT ( 'NONE',  ( -91.59502366432084841, 95.97275144416944670, -60.91270374391781672 ) ) ;
#7591 = ORIENTED_EDGE ( 'NONE', *, *, #1086, .T. ) ;
#7592 = CARTESIAN_POINT ( 'NONE',  ( 93.21002351426729149, 77.12912189496647386, 28.79774562292276840 ) ) ;
#7593 = ORIENTED_EDGE ( 'NONE', *, *, #13721, .T. ) ;
#7594 = CARTESIAN_POINT ( 'NONE',  ( 3.600951189929047391, 166.5359973580429482, 278.5988009334944877 ) ) ;
#7595 = CARTESIAN_POINT ( 'NONE',  ( -91.39645842968019451, 77.87428392844081770, -30.00278187767193927 ) ) ;
#7596 = DIRECTION ( 'NONE',  ( 0.01035335185279129787, 0.005513005182357351951, 0.9999312050732647172 ) ) ;
#7597 = CARTESIAN_POINT ( 'NONE',  ( -66.75560256528235925, 192.1022009597331817, 19.34154534151025118 ) ) ;
#7598 = VECTOR ( 'NONE', #20702, 1000.000000000000114 ) ;
#7599 = DIRECTION ( 'NONE',  ( -0.01292394549866632963, -0.005513023399716958026, -0.9999012842304692006 ) ) ;
#7600 = ADVANCED_FACE ( 'NONE', ( #3805 ), #14272, .T. ) ;
#7601 = DIRECTION ( 'NONE',  ( 0.01292414190464177652, 1.902755938799532355E-22, 0.9999164797902015955 ) ) ;
#7602 =( NAMED_UNIT ( * ) PLANE_ANGLE_UNIT ( ) SI_UNIT ( $, .RADIAN. ) );
#7603 = EDGE_CURVE ( 'NONE', #7438, #22518, #5191, .T. ) ;
#7604 = CARTESIAN_POINT ( 'NONE',  ( -64.64767546932813502, 126.1473081376430798, 27.67873648630093797 ) ) ;
#7605 = VERTEX_POINT ( 'NONE', #10927 ) ;
#7606 = DIRECTION ( 'NONE',  ( -0.9999164797902017066, -4.653667080246436871E-16, 0.01292414190464177999 ) ) ;
#7607 = ORIENTED_EDGE ( 'NONE', *, *, #13993, .F. ) ;
#7608 = ORIENTED_EDGE ( 'NONE', *, *, #8776, .F. ) ;
#7609 = CARTESIAN_POINT ( 'NONE',  ( -90.11843179045052921, 88.40872791604708425, 52.82837235832041500 ) ) ;
#7611 = ORIENTED_EDGE ( 'NONE', *, *, #3017, .F. ) ;
#7610 = ORIENTED_EDGE ( 'NONE', *, *, #14610, .F. ) ;
#7612 = AXIS2_PLACEMENT_3D ( 'NONE', #22432, #12010, #21884 ) ;
#7613 = CARTESIAN_POINT ( 'NONE',  ( 39.53412429657601734, 95.80343351084772507, -43.21010328702048042 ) ) ;
#7614 = CARTESIAN_POINT ( 'NONE',  ( -56.11381622223437660, 118.5884715842524315, 107.6180086640604543 ) ) ;
#7615 = CARTESIAN_POINT ( 'NONE',  ( -90.15711184568681347, 79.46353706204938305, -27.61532001585845109 ) ) ;
#7616 = CARTESIAN_POINT ( 'NONE',  ( 70.44022362938051174, 70.80424004364375890, 84.48783506240397401 ) ) ;
#7617 = EDGE_LOOP ( 'NONE', ( #2942, #4224, #6476 ) ) ;
#7618 = CARTESIAN_POINT ( 'NONE',  ( 48.50680475866421659, 162.7171858343479016, 268.0384508536055819 ) ) ;
#7619 = CARTESIAN_POINT ( 'NONE',  ( 19.60796286561798496, 183.9592037085494383, 312.5281987576885854 ) ) ;
#7620 = CARTESIAN_POINT ( 'NONE',  ( 92.63973831233896306, 79.05196971970121922, 26.25410855708543423 ) ) ;
#7621 = CARTESIAN_POINT ( 'NONE',  ( -92.82229925712802299, 69.99999999999998579, 1.199748770783236385 ) ) ;
#7622 = ORIENTED_EDGE ( 'NONE', *, *, #7712, .F. ) ;
#7623 = VECTOR ( 'NONE', #579, 1000.000000000000000 ) ;
#7624 = FACE_OUTER_BOUND ( 'NONE', #2379, .T. ) ;
#7625 = DIRECTION ( 'NONE',  ( 0.9999164797902015955, 6.965998958219364448E-18, -0.01292414190464157182 ) ) ;
#7626 = ORIENTED_EDGE ( 'NONE', *, *, #5534, .F. ) ;
#7627 = DIRECTION ( 'NONE',  ( 0.01111468050521610164, -0.5103046645782707280, 0.8599218645824314722 ) ) ;
#7628 = ORIENTED_EDGE ( 'NONE', *, *, #16977, .T. ) ;
#7629 = VECTOR ( 'NONE', #294, 1000.000000000000114 ) ;
#7630 = CARTESIAN_POINT ( 'NONE',  ( 75.07439005099489293, 75.00866199770877074, 0.3533726697390237592 ) ) ;
#7631 = CARTESIAN_POINT ( 'NONE',  ( -90.49431781703050603, 70.72571308208034679, 61.29990699711781588 ) ) ;
#7632 = EDGE_LOOP ( 'NONE', ( #5022, #11471, #19064, #14426 ) ) ;
#7633 = DIRECTION ( 'NONE',  ( 0.9909299940865186063, -0.1338359446631180727, -0.01207007604876311237 ) ) ;
#7634 = CARTESIAN_POINT ( 'NONE',  ( 11.93221611429111384, 159.4520312983160295, 323.8685343595495851 ) ) ;
#7635 = AXIS2_PLACEMENT_3D ( 'NONE', #11358, #5834, #11016 ) ;
#7636 = LINE ( 'NONE', #2598, #20650 ) ;
#7637 = ORIENTED_EDGE ( 'NONE', *, *, #4152, .T. ) ;
#7638 = DIRECTION ( 'NONE',  ( 0.9232306267972776315, 0.000000000000000000, -0.3842462878721224495 ) ) ;
#7639 = DIRECTION ( 'NONE',  ( 0.7861822061943918305, 8.225665855602111769E-19, 0.6179947723592160713 ) ) ;
#7640 = DIRECTION ( 'NONE',  ( 0.01292394549866738955, 0.005513023399720468239, 0.9999012842304693116 ) ) ;
#7641 = CARTESIAN_POINT ( 'NONE',  ( -41.44918043768936400, 158.5452755494390544, 269.2241539901819465 ) ) ;
#7642 = CARTESIAN_POINT ( 'NONE',  ( -9.736871716074000815, 187.7457344247829667, 321.1662588281238868 ) ) ;
#7644 = DIRECTION ( 'NONE',  ( -2.025474946048326158E-22, 1.000000000000000000, -1.876735158486679638E-22 ) ) ;
#7643 = DIRECTION ( 'NONE',  ( 0.4910069343201003411, -0.004767316193522950878, -0.8711426192914036859 ) ) ;
#7645 = DIRECTION ( 'NONE',  ( -2.459148776293844314E-24, 1.000000000000000000, -1.902597020224326827E-22 ) ) ;
#7646 = ORIENTED_EDGE ( 'NONE', *, *, #16709, .T. ) ;
#7647 = EDGE_CURVE ( 'NONE', #13728, #8873, #20964, .T. ) ;
#7648 = CARTESIAN_POINT ( 'NONE',  ( -41.00000899811524846, 169.5540992312279229, 273.1580453575298293 ) ) ;
#7649 = EDGE_CURVE ( 'NONE', #17163, #18513, #5854, .T. ) ;
#7650 = ORIENTED_EDGE ( 'NONE', *, *, #13505, .F. ) ;
#7651 = DIRECTION ( 'NONE',  ( 7.125109674161246868E-05, -0.9999848031710252272, 0.005512562950850154186 ) ) ;
#7652 = CARTESIAN_POINT ( 'NONE',  ( -10.92760325396984022, 186.9328588273032210, 308.3314949570851127 ) ) ;
#7653 = AXIS2_PLACEMENT_3D ( 'NONE', #383, #7378, #13043 ) ;
#7654 = ORIENTED_EDGE ( 'NONE', *, *, #16525, .F. ) ;
#7655 = ORIENTED_EDGE ( 'NONE', *, *, #15264, .F. ) ;
#7656 = DIRECTION ( 'NONE',  ( 7.125109674160325297E-05, -0.9999848031710253382, 0.005512562950849327591 ) ) ;
#7657 = B_SPLINE_CURVE_WITH_KNOTS ( 'NONE', 3,
 ( #11770, #15241, #20595, #10045, #6378, #18650, #15460, #13834, #2914, #4732, #22196, #22414, #20474, #3369, #10386, #1091 ),
 .UNSPECIFIED., .F., .F.,
 ( 4, 2, 2, 2, 2, 2, 2, 4 ),
 ( 0.000000000000000000, 0.0004288218673305856272, 0.0008576437346611712545, 0.001286465601991756882, 0.001715287469322342509, 0.002144109336652928136, 0.002572931203983513763, 0.003430574938644721447 ),
 .UNSPECIFIED. ) ;
#7658 = CARTESIAN_POINT ( 'NONE',  ( 12.03061627106288967, 188.3248577112672706, 306.6667676847338271 ) ) ;
#7659 = EDGE_CURVE ( 'NONE', #5759, #22007, #597, .T. ) ;
#7660 = ITEM_DEFINED_TRANSFORMATION ( 'NONE', 'NONE', #18,  #6292 ) ;
#7661 = EDGE_CURVE ( 'NONE', #18024, #6487, #13665, .T. ) ;
#7662 = CONICAL_SURFACE ( 'NONE', #14669, 11.00000000000000178, 0.7853981633974346233 ) ;
#7663 = ORIENTED_EDGE ( 'NONE', *, *, #6175, .T. ) ;
#7664 = LINE ( 'NONE', #20061, #7442 ) ;
#7665 = EDGE_CURVE ( 'NONE', #12549, #17825, #14621, .T. ) ;
#7666 = AXIS2_PLACEMENT_3D ( 'NONE', #21679, #16448, #2302 ) ;
#7667 = LINE ( 'NONE', #18251, #14064 ) ;
#7668 = VERTEX_POINT ( 'NONE', #3679 ) ;
#7669 = B_SPLINE_CURVE_WITH_KNOTS ( 'NONE', 3,
 ( #15527, #15642, #8481, #22363, #6771, #4806, #17474, #3100, #1724, #1615, #17585, #4789, #22586, #3199, #13564, #8374 ),
 .UNSPECIFIED., .F., .F.,
 ( 4, 2, 2, 2, 2, 2, 2, 4 ),
 ( 6.691626947686431882E-17, 0.0003925140011974886174, 0.0007850280023949103396, 0.001177542003592332333, 0.001570056004789753892, 0.001962570005987175452, 0.002355084007184597445, 0.003140112009579444901 ),
 .UNSPECIFIED. ) ;
#7670 = EDGE_LOOP ( 'NONE', ( #16502, #3473, #3074, #9546 ) ) ;
#7671 = DIRECTION ( 'NONE',  ( 0.01292394549866739996, 0.005513023399721131770, 0.9999012842304692006 ) ) ;
#7672 = PLANE ( 'NONE',  #13584 ) ;
#7673 = ORIENTED_EDGE ( 'NONE', *, *, #3759, .F. ) ;
#7674 = CARTESIAN_POINT ( 'NONE',  ( -59.45646666158516780, 114.2347186777957830, 170.4837605623661148 ) ) ;
#7675 = ORIENTED_EDGE ( 'NONE', *, *, #18129, .T. ) ;
#7676 = CARTESIAN_POINT ( 'NONE',  ( -11.14759061400257423, 137.5759562808229362, 104.7141423461399086 ) ) ;
#7677 = CARTESIAN_POINT ( 'NONE',  ( 1.054933926688728762, 165.4499317482979279, 81.61824794009152129 ) ) ;
#7678 = LINE ( 'NONE', #14719, #14773 ) ;
#7679 = ORIENTED_EDGE ( 'NONE', *, *, #11556, .T. ) ;
#7680 = EDGE_CURVE ( 'NONE', #20021, #14769, #16119, .T. ) ;
#7681 = B_SPLINE_CURVE_WITH_KNOTS ( 'NONE', 3,
 ( #21591, #9432, #14416, #14637, #5649, #16473 ),
 .UNSPECIFIED., .F., .F.,
 ( 4, 2, 4 ),
 ( 0.01452727543195645940, 0.01715716534226981171, 0.01978705525258316056 ),
 .UNSPECIFIED. ) ;
#7682 = EDGE_CURVE ( 'NONE', #3399, #5284, #11613, .T. ) ;
#7683 = CARTESIAN_POINT ( 'NONE',  ( 36.15575925104655397, 93.60246426260026453, 82.12095663381342092 ) ) ;
#7684 = AXIS2_PLACEMENT_3D ( 'NONE', #7248, #14628, #16019 ) ;
#7685 = AXIS2_PLACEMENT_3D ( 'NONE', #13412, #11790, #22429 ) ;
#7686 = CARTESIAN_POINT ( 'NONE',  ( -64.64902924016615771, 145.1470193978925636, 27.57399779023469932 ) ) ;
#7687 = AXIS2_PLACEMENT_3D ( 'NONE', #19033, #3767, #8461 ) ;
#7688 = ORIENTED_EDGE ( 'NONE', *, *, #9835, .T. ) ;
#7689 = B_SPLINE_CURVE_WITH_KNOTS ( 'NONE', 3,
 ( #14678, #13073, #7877, #20037, #4190, #13176, #21630, #2249, #20141, #5919, #14917, #4411, #2717, #12955, #12719, #11220, #9250, #19686, #18227, #3955, #10978, #539, #18006, #8317, #18778, #1230, #11901, #15015, #10278, #13510, #20607, #2924, #6268, #20269, #10163, #13740, #15358, #20487, #20723, #4640, #22306, #4975, #16969 ),
 .UNSPECIFIED., .F., .F.,
 ( 4, 2, 2, 1, 2, 2, 2, 2, 2, 2, 2, 2, 2, 2, 2, 2, 2, 2, 2, 2, 2, 4 ),
 ( 0.01954562671941673449, 0.02076694801418337011, 0.02137760866156668618, 0.02198826930895000573, 0.02259892995633332180, 0.02320959060371664134, 0.02443091189848327349, 0.02565223319324991258, 0.02687355448801654473, 0.02748421513539988509, 0.02809487578278321851, 0.02931619707754989229, 0.03053751837231656954, 0.03114817901969990643, 0.03175883966708323985, 0.03298016096184991364, 0.03420148225661659436, 0.03542280355138326120, 0.03603346419876658768, 0.03664412484614991417, 0.03786544614091655325, 0.03908676743568318540 ),
 .UNSPECIFIED. ) ;
#7690 = CARTESIAN_POINT ( 'NONE',  ( -93.23587179807654479, 72.00000000000000000, -30.79757858250321689 ) ) ;
#7691 = CARTESIAN_POINT ( 'NONE',  ( -88.41179892586471567, 88.71926944898528689, 50.32451584197536221 ) ) ;
#7692 = ADVANCED_FACE ( 'NONE', ( #9418 ), #20087, .T. ) ;
#7693 = EDGE_LOOP ( 'NONE', ( #1663, #3913 ) ) ;
#7694 = DIRECTION ( 'NONE',  ( 0.000000000000000000, 0.000000000000000000, -1.000000000000000000 ) ) ;
#7695 = EDGE_CURVE ( 'NONE', #3576, #719, #8159, .T. ) ;
#7696 = VERTEX_POINT ( 'NONE', #6331 ) ;
#7697 = CARTESIAN_POINT ( 'NONE',  ( 4.150218873619613724, 166.7703008525310793, 321.0946055132897072 ) ) ;
#7698 = DIRECTION ( 'NONE',  ( 0.9999164797902015955, 0.000000000000000000, -0.01292414190464118845 ) ) ;
#7699 = ORIENTED_EDGE ( 'NONE', *, *, #19417, .F. ) ;
#7700 = VECTOR ( 'NONE', #21554, 1000.000000000000114 ) ;
#7701 = CARTESIAN_POINT ( 'NONE',  ( 8.306869994213354147, 188.3716244831220479, 274.4171887809970940 ) ) ;
#7702 = PRODUCT ( 'Movable Vise Jaw Block', 'Movable Vise Jaw Block', '', ( #13552 ) ) ;
#7703 = AXIS2_PLACEMENT_3D ( 'NONE', #16490, #9582, #2456 ) ;
#7704 = DIRECTION ( 'NONE',  ( -0.01292414190465215537, 0.000000000000000000, -0.9999164797902015955 ) ) ;
#7705 = EDGE_LOOP ( 'NONE', ( #7234, #16577, #7922, #15242 ) ) ;
#7706 = CARTESIAN_POINT ( 'NONE',  ( 26.52201511833298397, 169.3335548213015329, 322.2914605072682548 ) ) ;
#7707 = ORIENTED_EDGE ( 'NONE', *, *, #3005, .F. ) ;
#7708 = CARTESIAN_POINT ( 'NONE',  ( -72.65623182917823897, 87.80665977804258659, 70.23323934248251987 ) ) ;
#7709 = CARTESIAN_POINT ( 'NONE',  ( 49.14156507091730930, 189.5933979181235998, -74.44835251036772661 ) ) ;
#7710 = DIRECTION ( 'NONE',  ( 7.125109674403838460E-05, -0.9999848031710254492, 0.005512562950847868688 ) ) ;
#7711 = DIRECTION ( 'NONE',  ( 0.009760756503428008254, -0.9999378516499564107, 0.005387065077611006073 ) ) ;
#7712 = EDGE_CURVE ( 'NONE', #13823, #22174, #6444, .T. ) ;
#7713 = DIRECTION ( 'NONE',  ( 0.009760756503428037745, -0.9999378516499562997, 0.005387065077612779827 ) ) ;
#7714 = ADVANCED_FACE ( 'NONE', ( #22026 ), #7928, .F. ) ;
#7715 = VERTEX_POINT ( 'NONE', #13018 ) ;
#7716 = DIRECTION ( 'NONE',  ( -0.01104128644981280764, -0.5197558313507618655, -0.8542435049623797738 ) ) ;
#7717 = LINE ( 'NONE', #3921, #10458 ) ;
#7718 = AXIS2_PLACEMENT_3D ( 'NONE', #13664, #22340, #6638 ) ;
#7719 = DIRECTION ( 'NONE',  ( -0.01292414190464131508, 0.000000000000000000, -0.9999164797902017066 ) ) ;
#7720 = VERTEX_POINT ( 'NONE', #2867 ) ;
#7721 = DIRECTION ( 'NONE',  ( -7.125109674160258889E-05, 0.9999848031710252272, -0.005512562950849897447 ) ) ;
#7722 = ORIENTED_EDGE ( 'NONE', *, *, #1491, .T. ) ;
#7723 = VECTOR ( 'NONE', #19458, 999.9999999999998863 ) ;
#7724 = EDGE_LOOP ( 'NONE', ( #21643, #2918, #3898, #14974 ) ) ;
#7725 = CARTESIAN_POINT ( 'NONE',  ( -82.31274079517788778, 75.11017898543126137, -3.511195801982965214 ) ) ;
#7726 = CIRCLE ( 'NONE', #763, 3.399999999999992806 ) ;
#7727 = CARTESIAN_POINT ( 'NONE',  ( -90.13867034150928248, 88.25703757669403160, 52.94586342302623194 ) ) ;
#7728 = AXIS2_PLACEMENT_3D ( 'NONE', #9197, #12552, #147 ) ;
#7729 = AXIS2_PLACEMENT_3D ( 'NONE', #18328, #7639, #3959 ) ;
#7730 = ORIENTED_EDGE ( 'NONE', *, *, #3610, .F. ) ;
#7731 = EDGE_CURVE ( 'NONE', #9852, #9497, #17723, .T. ) ;
#7732 = LINE ( 'NONE', #4710, #4802 ) ;
#7733 = CIRCLE ( 'NONE', #16192, 3.399999999999985700 ) ;
#7734 = EDGE_CURVE ( 'NONE', #8312, #15577, #19977, .T. ) ;
#7735 = DIRECTION ( 'NONE',  ( -0.01292414190464132896, 0.000000000000000000, -0.9999164797902015955 ) ) ;
#7736 = CARTESIAN_POINT ( 'NONE',  ( -4.313798532395376917, 189.6286013151541283, 275.0874112264361884 ) ) ;
#7737 = CARTESIAN_POINT ( 'NONE',  ( -35.92446336679493157, 93.51775827232350480, -82.02042234242476582 ) ) ;
#7738 = CARTESIAN_POINT ( 'NONE',  ( -37.38783854551962804, 93.14158652660637472, 85.23980647655857013 ) ) ;
#7739 = DIRECTION ( 'NONE',  ( 7.125109674364536131E-05, -0.9999848031710253382, 0.005512562950849705760 ) ) ;
#7740 = CARTESIAN_POINT ( 'NONE',  ( 19.50026166618112100, 184.8320841190834756, 278.1813969851201023 ) ) ;
#7741 = CARTESIAN_POINT ( 'NONE',  ( 20.32472999537270653, 182.3369386323682875, 317.0014608700818144 ) ) ;
#7742 = B_SPLINE_CURVE_WITH_KNOTS ( 'NONE', 3,
 ( #18669, #13419, #4541, #15262, #11569, #9618, #22212, #2828, #2934, #9953, #20494, #21756, #3694, #4875 ),
 .UNSPECIFIED., .F., .F.,
 ( 4, 2, 2, 2, 2, 2, 4 ),
 ( 0.000000000000000000, 0.001119727475084554861, 0.001679591212626828714, 0.002239454950169102784, 0.003359182425253666102, 0.003919046162795954483, 0.004478909900338241996 ),
 .UNSPECIFIED. ) ;
#7743 = CARTESIAN_POINT ( 'NONE',  ( -19.00908416305977156, 180.4221386788646271, 76.79453591276953262 ) ) ;
#7744 = AXIS2_PLACEMENT_3D ( 'NONE', #20308, #607, #5870 ) ;
#7745 = AXIS2_PLACEMENT_3D ( 'NONE', #20956, #64, #2019 ) ;
#7746 = DIRECTION ( 'NONE',  ( 1.387778780781445676E-14, 0.000000000000000000, 1.000000000000000000 ) ) ;
#7747 =( GEOMETRIC_REPRESENTATION_CONTEXT ( 3 ) GLOBAL_UNCERTAINTY_ASSIGNED_CONTEXT ( ( #7917 ) ) GLOBAL_UNIT_ASSIGNED_CONTEXT ( ( #7908, #8139, #11252 ) ) REPRESENTATION_CONTEXT ( 'NONE', 'WORKASPACE' ) );
#7748 = ORIENTED_EDGE ( 'NONE', *, *, #10071, .F. ) ;
#7749 = DIRECTION ( 'NONE',  ( -0.9999164797902017066, -6.965998958219365988E-18, 0.01292414190464157356 ) ) ;
#7750 = AXIS2_PLACEMENT_3D ( 'NONE', #19933, #22191, #1326 ) ;
#7751 = DIRECTION ( 'NONE',  ( -0.5617652846616787432, -0.7071067811865489050, -0.4294412240912379164 ) ) ;
#7752 = ORIENTED_EDGE ( 'NONE', *, *, #9207, .F. ) ;
#7753 = DIRECTION ( 'NONE',  ( -0.006350819331212799977, 0.8709385446395345731, -0.4913509118287983091 ) ) ;
#7754 = ORIENTED_EDGE ( 'NONE', *, *, #17676, .T. ) ;
#7755 = CARTESIAN_POINT ( 'NONE',  ( -22.25632012706247664, 95.51270090492249665, 81.95880486798408526 ) ) ;
#7756 = EDGE_CURVE ( 'NONE', #13377, #3120, #4108, .T. ) ;
#7757 = DIRECTION ( 'NONE',  ( 7.125109674403837105E-05, -0.9999848031710252272, 0.005512562950847867821 ) ) ;
#7758 =( GEOMETRIC_REPRESENTATION_CONTEXT ( 3 ) GLOBAL_UNCERTAINTY_ASSIGNED_CONTEXT ( ( #13837 ) ) GLOBAL_UNIT_ASSIGNED_CONTEXT ( ( #17274, #11652, #3135 ) ) REPRESENTATION_CONTEXT ( 'NONE', 'WORKASPACE' ) );
#7759 = CARTESIAN_POINT ( 'NONE',  ( 77.38145957316694989, 75.10270664613308611, -5.417547979167955496 ) ) ;
#7760 = CARTESIAN_POINT ( 'NONE',  ( 0.000000000000000000, 37.00000000000000711, 0.000000000000000000 ) ) ;
#7761 = AXIS2_PLACEMENT_3D ( 'NONE', #11746, #3349, #13587 ) ;
#7762 = CARTESIAN_POINT ( 'NONE',  ( 17.14168828271968437, 177.4876913356084174, 88.22687136455920154 ) ) ;
#7763 = DIRECTION ( 'NONE',  ( 0.01292394549866738608, 0.005513023399720468239, 0.9999012842304692006 ) ) ;
#7764 = CIRCLE ( 'NONE', #6660, 10.99999999999999822 ) ;
#7765 = ORIENTED_EDGE ( 'NONE', *, *, #1491, .F. ) ;
#7766 = CARTESIAN_POINT ( 'NONE',  ( -69.24448582912822303, 92.41827837429551096, 85.47053766693683485 ) ) ;
#7767 = DIRECTION ( 'NONE',  ( 1.000000000000000000, 0.000000000000000000, 0.000000000000000000 ) ) ;
#7768 = CARTESIAN_POINT ( 'NONE',  ( 89.11130500643436392, 98.76544454674674967, -64.49243618084513230 ) ) ;
#7769 = DIRECTION ( 'NONE',  ( 0.9909299940865187173, -0.1338359446631179062, -0.01207007604876208194 ) ) ;
#7770 = CARTESIAN_POINT ( 'NONE',  ( 91.40469917791151033, 79.08369667522882196, -28.73783386972092302 ) ) ;
#7771 = CARTESIAN_POINT ( 'NONE',  ( 79.99331838321626265, 55.99999999999999289, 4.966068647628683053 ) ) ;
#7772 = CARTESIAN_POINT ( 'NONE',  ( -45.49127566601020334, 166.5779480061062827, 268.8320707926027922 ) ) ;
#7773 = SURFACE_SIDE_STYLE ('',( #4730 ) ) ;
#7774 = EDGE_LOOP ( 'NONE', ( #6799, #15090, #16957, #286, #187 ) ) ;
#7775 = CARTESIAN_POINT ( 'NONE',  ( 48.82981265512304248, 189.4975199778058368, -91.83668375125502337 ) ) ;
#7776 = AXIS2_PLACEMENT_3D ( 'NONE', #3212, #17248, #15088 ) ;
#7777 = FACE_OUTER_BOUND ( 'NONE', #13590, .T. ) ;
#7778 = CARTESIAN_POINT ( 'NONE',  ( -14.46581794479437910, 179.5756009467052365, 311.6243789545613367 ) ) ;
#7779 = VERTEX_POINT ( 'NONE', #18278 ) ;
#7780 = CIRCLE ( 'NONE', #2635, 110.0000000000000000 ) ;
#7781 = VERTEX_POINT ( 'NONE', #14741 ) ;
#7782 = CARTESIAN_POINT ( 'NONE',  ( -71.88056509240439595, 96.34227735399929315, 78.69877631277590524 ) ) ;
#7783 = APPLICATION_CONTEXT ( 'automotive_design' ) ;
#7784 = FACE_OUTER_BOUND ( 'NONE', #16108, .T. ) ;
#7785 = CIRCLE ( 'NONE', #1563, 110.0000000000000000 ) ;
#7786 = EDGE_CURVE ( 'NONE', #7720, #12921, #20427, .T. ) ;
#7787 = ORIENTED_EDGE ( 'NONE', *, *, #22205, .F. ) ;
#7788 = AXIS2_PLACEMENT_3D ( 'NONE', #17814, #13887, #15739 ) ;
#7789 = AXIS2_PLACEMENT_3D ( 'NONE', #538, #6361, #19685 ) ;
#7790 = LINE ( 'NONE', #11243, #5599 ) ;
#7791 = DIRECTION ( 'NONE',  ( 0.01292414190464131508, 0.000000000000000000, 0.9999164797902017066 ) ) ;
#7792 = ORIENTED_EDGE ( 'NONE', *, *, #11262, .T. ) ;
#7793 = ORIENTED_EDGE ( 'NONE', *, *, #11607, .F. ) ;
#7794 = CARTESIAN_POINT ( 'NONE',  ( -48.56932532720185947, 144.7550503794368524, -43.73743426306185000 ) ) ;
#7795 = ORIENTED_EDGE ( 'NONE', *, *, #5316, .F. ) ;
#7796 = CARTESIAN_POINT ( 'NONE',  ( -13.25750401672744161, 181.1680438727101432, 307.7338533305215833 ) ) ;
#7797 = AXIS2_PLACEMENT_3D ( 'NONE', #9538, #22147, #939 ) ;
#7798 = ORIENTED_EDGE ( 'NONE', *, *, #9691, .F. ) ;
#7799 = CARTESIAN_POINT ( 'NONE',  ( 55.40268456415110165, 1.999999999999998224, 113.1659955246503415 ) ) ;
#7800 = CARTESIAN_POINT ( 'NONE',  ( -163.1715728752537871, -6.488953147413177264E-16, -8.828427124746170307 ) ) ;
#7801 = CARTESIAN_POINT ( 'NONE',  ( 1.054933926688728762, 165.4499317482979279, 81.61824794009152129 ) ) ;
#7802 = CARTESIAN_POINT ( 'NONE',  ( -42.56847267762256593, 125.7553391191873544, -43.71024041842355246 ) ) ;
#7803 = VERTEX_POINT ( 'NONE', #11378 ) ;
#7804 = ADVANCED_FACE ( 'NONE', ( #828 ), #4491, .T. ) ;
#7805 = DIRECTION ( 'NONE',  ( -0.9999164797902015955, -2.044556590511377167E-15, 0.01292414190464178346 ) ) ;
#7806 = ADVANCED_FACE ( 'NONE', ( #21800 ), #11716, .F. ) ;
#7807 = CIRCLE ( 'NONE', #19539, 7.499999999999991118 ) ;
#7808 = VECTOR ( 'NONE', #5751, 999.9999999999998863 ) ;
#7809 = CARTESIAN_POINT ( 'NONE',  ( -8.671153205961791954, 185.7650231504708529, 306.6267288985166601 ) ) ;
#7810 = ADVANCED_FACE ( 'NONE', ( #2658 ), #11844, .T. ) ;
#7811 = ORIENTED_EDGE ( 'NONE', *, *, #20019, .F. ) ;
#7812 = CARTESIAN_POINT ( 'NONE',  ( -55.40268456415261511, 1.999999999999998224, 113.1659955246496025 ) ) ;
#7813 = CARTESIAN_POINT ( 'NONE',  ( -89.57008079183799509, 88.24871054370684931, 50.63090528479802543 ) ) ;
#7814 = SHAPE_DEFINITION_REPRESENTATION ( #2770, #7092 ) ;
#7815 = EDGE_CURVE ( 'NONE', #20064, #15219, #20204, .T. ) ;
#7816 = ORIENTED_EDGE ( 'NONE', *, *, #12891, .F. ) ;
#7817 = EDGE_CURVE ( 'NONE', #3254, #4632, #18506, .T. ) ;
#7818 = CARTESIAN_POINT ( 'NONE',  ( -49.75187073772171686, 112.0017951520220123, -43.54156231249048403 ) ) ;
#7819 = ORIENTED_EDGE ( 'NONE', *, *, #18193, .T. ) ;
#7820 = DIRECTION ( 'NONE',  ( 0.000000000000000000, 0.000000000000000000, 1.000000000000000000 ) ) ;
#7821 = DIRECTION ( 'NONE',  ( -7.125109674403837105E-05, 0.9999848031710252272, -0.005512562950847867821 ) ) ;
#7822 = ORIENTED_EDGE ( 'NONE', *, *, #4737, .F. ) ;
#7823 = CIRCLE ( 'NONE', #16299, 3.047499999999998987 ) ;
#7824 = EDGE_CURVE ( 'NONE', #12220, #19868, #16790, .T. ) ;
#7825 = DIRECTION ( 'NONE',  ( -0.01292394549866738608, -0.005513023399720698957, -0.9999012842304692006 ) ) ;
#7826 = CIRCLE ( 'NONE', #20652, 4.500000000000006217 ) ;
#7827 = CARTESIAN_POINT ( 'NONE',  ( -44.75576560912451640, 168.6025580852140706, 19.18675944895310082 ) ) ;
#7828 = VERTEX_POINT ( 'NONE', #8034 ) ;
#7829 = CARTESIAN_POINT ( 'NONE',  ( -41.00000899811524846, 169.5540992312279229, 273.1580453575298293 ) ) ;
#7830 = ORIENTED_EDGE ( 'NONE', *, *, #10582, .T. ) ;
#7831 = DIRECTION ( 'NONE',  ( -0.01292394549866731669, -0.005513023399720593139, -0.9999012842304692006 ) ) ;
#7832 = FACE_OUTER_BOUND ( 'NONE', #18394, .T. ) ;
#7833 = CYLINDRICAL_SURFACE ( 'NONE', #17545, 6.000000000000000888 ) ;
#7834 = DIRECTION ( 'NONE',  ( 0.01292394549866743812, 0.005513023399720639109, 0.9999012842304693116 ) ) ;
#7835 = EDGE_CURVE ( 'NONE', #19083, #13764, #7055, .T. ) ;
#7836 = ORIENTED_EDGE ( 'NONE', *, *, #3343, .F. ) ;
#7837 = FACE_BOUND ( 'NONE', #4007, .T. ) ;
#7838 =( NAMED_UNIT ( * ) PLANE_ANGLE_UNIT ( ) SI_UNIT ( $, .RADIAN. ) );
#7839 = AXIS2_PLACEMENT_3D ( 'NONE', #4980, #6602, #18997 ) ;
#7840 = CARTESIAN_POINT ( 'NONE',  ( -154.0000000000000000, 1.999999999999998224, -53.76161406891256433 ) ) ;
#7841 = EDGE_LOOP ( 'NONE', ( #5258, #733, #4558, #602 ) ) ;
#7842 = DIRECTION ( 'NONE',  ( -0.9999164797902015955, -2.001050586450178695E-22, 0.01292414190464131335 ) ) ;
#7843 = EDGE_CURVE ( 'NONE', #5091, #11676, #8884, .T. ) ;
#7844 = ORIENTED_EDGE ( 'NONE', *, *, #4413, .T. ) ;
#7845 = AXIS2_PLACEMENT_3D ( 'NONE', #3715, #17984, #12699 ) ;
#7846 = VERTEX_POINT ( 'NONE', #21002 ) ;
#7847 = ORIENTED_EDGE ( 'NONE', *, *, #292, .F. ) ;
#7848 = AXIS2_PLACEMENT_3D ( 'NONE', #3495, #8540, #10852 ) ;
#7849 = CARTESIAN_POINT ( 'NONE',  ( -105.2816027134186641, 70.66149885336977832, 31.87151722101068430 ) ) ;
#7850 = CARTESIAN_POINT ( 'NONE',  ( 13.76389349044818644, 189.8999012668466833, 307.9600247906288928 ) ) ;
#7851 = ORIENTED_EDGE ( 'NONE', *, *, #17991, .T. ) ;
#7852 = EDGE_CURVE ( 'NONE', #3099, #6325, #19884, .T. ) ;
#7853 = CARTESIAN_POINT ( 'NONE',  ( -71.57228119427200852, 96.47114962407205496, 78.56582497698298084 ) ) ;
#7854 = CYLINDRICAL_SURFACE ( 'NONE', #17574, 4.000000000000002665 ) ;
#7855 = AXIS2_PLACEMENT_3D ( 'NONE', #19317, #7252, #6801 ) ;
#7856 = DIRECTION ( 'NONE',  ( -7.125109674161246868E-05, 0.9999848031710252272, -0.005512562950850154186 ) ) ;
#7857 = CARTESIAN_POINT ( 'NONE',  ( -16.68277397329964273, 181.4144828908143552, 256.7767670742539963 ) ) ;
#7858 = VERTEX_POINT ( 'NONE', #8366 ) ;
#7859 = CARTESIAN_POINT ( 'NONE',  ( 20.69885819030740493, 181.8884547447338207, 314.5091122468493268 ) ) ;
#7860 = VECTOR ( 'NONE', #3627, 1000.000000000000114 ) ;
#7861 = DIRECTION ( 'NONE',  ( 7.125109674161238737E-05, -0.9999848031710253382, 0.005512562950850163727 ) ) ;
#7862 = AXIS2_PLACEMENT_3D ( 'NONE', #1597, #103, #8586 ) ;
#7863 = LINE ( 'NONE', #7621, #21991 ) ;
#7864 = EDGE_CURVE ( 'NONE', #7432, #20838, #95, .T. ) ;
#7865 = CARTESIAN_POINT ( 'NONE',  ( -46.77184957787964237, 141.3748088146942621, 250.0790257996952164 ) ) ;
#7866 = CARTESIAN_POINT ( 'NONE',  ( -9.065023647928146744, 109.7167603697149474, 130.3064260814875013 ) ) ;
#7867 = ORIENTED_EDGE ( 'NONE', *, *, #3164, .F. ) ;
#7868 = AXIS2_PLACEMENT_3D ( 'NONE', #3633, #17556, #13769 ) ;
#7869 = FACE_OUTER_BOUND ( 'NONE', #2872, .T. ) ;
#7870 = ORIENTED_EDGE ( 'NONE', *, *, #21564, .F. ) ;
#7871 = LINE ( 'NONE', #640, #914 ) ;
#7872 = CIRCLE ( 'NONE', #7376, 110.0000000000000000 ) ;
#7873 = CIRCLE ( 'NONE', #10091, 2.000000000000004885 ) ;
#7874 = ORIENTED_EDGE ( 'NONE', *, *, #19748, .F. ) ;
#7875 = ADVANCED_FACE ( 'NONE', ( #4800 ), #5256, .T. ) ;
#7876 = LINE ( 'NONE', #16297, #5420 ) ;
#7877 = CARTESIAN_POINT ( 'NONE',  ( 73.79388979939501780, 75.00262671344128762, -0.1404264124762290289 ) ) ;
#7878 = DIRECTION ( 'NONE',  ( -5.440186201345785633E-18, -1.000000000000000000, -1.334940939666367878E-17 ) ) ;
#7879 = DIRECTION ( 'NONE',  ( 0.9999164797902015955, 6.965998958219364448E-18, -0.01292414190464157182 ) ) ;
#7880 = ORIENTED_EDGE ( 'NONE', *, *, #12390, .T. ) ;
#7881 = CARTESIAN_POINT ( 'NONE',  ( 9.839100211760563042, 190.0747034078442539, 274.8007098013740688 ) ) ;
#7882 = CARTESIAN_POINT ( 'NONE',  ( -80.08460380590139494, -0.7076046073270642056, -127.3251198009944005 ) ) ;
#7883 = CARTESIAN_POINT ( 'NONE',  ( -44.26142469380095434, 168.8134312302532862, 57.43298357076854899 ) ) ;
#7884 = CARTESIAN_POINT ( 'NONE',  ( -40.56829007148257205, 106.8542505984647306, 71.50644046503228424 ) ) ;
#7885 = CARTESIAN_POINT ( 'NONE',  ( 91.23603883849617091, 78.43035437438882695, 30.82342686631245243 ) ) ;
#7886 = CARTESIAN_POINT ( 'NONE',  ( -8.381044803055207382, 185.3405392432284202, 323.2524327434741167 ) ) ;
#7887 = PLANE ( 'NONE',  #21352 ) ;
#7888 = CARTESIAN_POINT ( 'NONE',  ( -1.163172771417702700, 69.99999999999998579, -89.99248318111824574 ) ) ;
#7889 = ORIENTED_EDGE ( 'NONE', *, *, #14984, .T. ) ;
#7890 = EDGE_CURVE ( 'NONE', #5077, #16867, #2980, .T. ) ;
#7891 = FACE_OUTER_BOUND ( 'NONE', #16841, .T. ) ;
#7892 = CARTESIAN_POINT ( 'NONE',  ( -11.36165660420419066, 186.4279686652184012, 308.4742914312953985 ) ) ;
#7893 = ADVANCED_FACE ( 'NONE', ( #3096 ), #21714, .F. ) ;
#7894 = ORIENTED_EDGE ( 'NONE', *, *, #4435, .T. ) ;
#7895 = ORIENTED_EDGE ( 'NONE', *, *, #3198, .T. ) ;
#7896 = CARTESIAN_POINT ( 'NONE',  ( 13.80509744631564750, 155.5569384583423300, 100.8921482990249956 ) ) ;
#7897 = AXIS2_PLACEMENT_3D ( 'NONE', #10813, #18048, #17715 ) ;
#7898 = CARTESIAN_POINT ( 'NONE',  ( 12.74721152739840058, 190.3162922845854439, 307.8428787392024333 ) ) ;
#7899 = ORIENTED_EDGE ( 'NONE', *, *, #18070, .F. ) ;
#7900 = PRODUCT_DEFINITION ( 'UNKNOWN', '', #11387, #20744 ) ;
#7901 = CARTESIAN_POINT ( 'NONE',  ( -52.99080075248789967, 169.5754971982215125, -76.32034350670481615 ) ) ;
#7902 = CARTESIAN_POINT ( 'NONE',  ( -41.67747345744908216, 165.9786531560170886, 257.1849355913342379 ) ) ;
#7903 = ORIENTED_EDGE ( 'NONE', *, *, #22451, .F. ) ;
#7904 = CARTESIAN_POINT ( 'NONE',  ( 12.69681717808449406, 190.5419464543700485, 307.8407304119797345 ) ) ;
#7905 = CARTESIAN_POINT ( 'NONE',  ( -12.01575389183062192, 182.4076787623453129, 322.7174846376778987 ) ) ;
#7906 = VERTEX_POINT ( 'NONE', #18710 ) ;
#7907 = DIRECTION ( 'NONE',  ( -2.025474946048326158E-22, 1.000000000000000000, -1.876735158486679638E-22 ) ) ;
#7908 =( LENGTH_UNIT ( ) NAMED_UNIT ( * ) SI_UNIT ( .MILLI., .METRE. ) );
#7909 = LINE ( 'NONE', #18690, #11914 ) ;
#7910 = VECTOR ( 'NONE', #16791, 1000.000000000000114 ) ;
#7911 = CARTESIAN_POINT ( 'NONE',  ( -23.03918042842984804, 89.37478006253336105, 78.76536267817510861 ) ) ;
#7912 = ORIENTED_EDGE ( 'NONE', *, *, #17252, .T. ) ;
#7913 = CARTESIAN_POINT ( 'NONE',  ( 158.3970384574715524, 18.00000000000000355, -62.74304228515679682 ) ) ;
#7914 = CARTESIAN_POINT ( 'NONE',  ( -0.5772765004791022836, 81.90747236817706778, -80.84070517186573568 ) ) ;
#7915 = DIRECTION ( 'NONE',  ( -0.9999164797902017066, 0.000000000000000000, 0.01292414190463832269 ) ) ;
#7916 = VERTEX_POINT ( 'NONE', #6979 ) ;
#7917 = UNCERTAINTY_MEASURE_WITH_UNIT (LENGTH_MEASURE( 1.000000000000000082E-05 ), #7908, 'distance_accuracy_value', 'NONE');
#7918 = CARTESIAN_POINT ( 'NONE',  ( -61.67516800463454985, 127.4153035195788561, 257.6560318593087686 ) ) ;
#7919 = CARTESIAN_POINT ( 'NONE',  ( -146.5000000000000000, 18.00000000000000355, 8.000000000000017764 ) ) ;
#7920 = SHAPE_DEFINITION_REPRESENTATION ( #19981, #21177 ) ;
#7921 = CONICAL_SURFACE ( 'NONE', #14185, 11.00000000000000178, 0.7853981633974346233 ) ;
#7922 = ORIENTED_EDGE ( 'NONE', *, *, #16418, .T. ) ;
#7923 = DIRECTION ( 'NONE',  ( -0.000000000000000000, -1.000000000000000000, 0.000000000000000000 ) ) ;
#7924 = ADVANCED_FACE ( 'NONE', ( #10112 ), #15303, .F. ) ;
#7925 = CARTESIAN_POINT ( 'NONE',  ( 90.50186546057696546, 78.02565673216736286, -32.58161589089097276 ) ) ;
#7926 = CARTESIAN_POINT ( 'NONE',  ( 13.43154693195699068, 190.0791210297336988, 320.8088049362866059 ) ) ;
#7927 = DIRECTION ( 'NONE',  ( -1.000000000000000000, 0.000000000000000000, 9.912705577010318154E-17 ) ) ;
#7928 = CYLINDRICAL_SURFACE ( 'NONE', #13329, 4.199999999999997513 ) ;
#7929 = EDGE_LOOP ( 'NONE', ( #8164, #1883, #17926, #20619 ) ) ;
#7930 = DIRECTION ( 'NONE',  ( 0.9999164797902017066, 6.965998958219365988E-18, -0.01292414190464157356 ) ) ;
#7931 = CARTESIAN_POINT ( 'NONE',  ( 68.81222610332000045, 91.74143318381845802, -85.81887827424428394 ) ) ;
#7932 = ORIENTED_EDGE ( 'NONE', *, *, #20290, .F. ) ;
#7933 = LINE ( 'NONE', #22033, #10633 ) ;
#7934 = ORIENTED_EDGE ( 'NONE', *, *, #12164, .F. ) ;
#7935 = CARTESIAN_POINT ( 'NONE',  ( 41.56623493000984126, 91.17157287525387233, 82.46967996629570052 ) ) ;
#7936 = CYLINDRICAL_SURFACE ( 'NONE', #15576, 2.000000000000004441 ) ;
#7937 = CARTESIAN_POINT ( 'NONE',  ( -56.11559749965279309, 143.5880916635282176, 107.4801945902891021 ) ) ;
#7938 = B_SPLINE_CURVE_WITH_KNOTS ( 'NONE', 3,
 ( #12519, #7983, #9483, #20146 ),
 .UNSPECIFIED., .F., .F.,
 ( 4, 4 ),
 ( 2.380735202048151846E-07, 0.002921157996826920233 ),
 .UNSPECIFIED. ) ;
#7939 = FACE_OUTER_BOUND ( 'NONE', #10560, .T. ) ;
#7940 = DIRECTION ( 'NONE',  ( -0.1296504907605108559, -0.005475273188901296634, -0.9915446392518419971 ) ) ;
#7941 = CYLINDRICAL_SURFACE ( 'NONE', #5310, 6.499999999999985789 ) ;
#7942 = EDGE_CURVE ( 'NONE', #6252, #11917, #20771, .T. ) ;
#7943 = EDGE_LOOP ( 'NONE', ( #21826, #8028, #1777, #8438 ) ) ;
#7944 = CARTESIAN_POINT ( 'NONE',  ( 12.84373220155140949, 190.4863343871390953, 307.8501923929725876 ) ) ;
#7945 = ADVANCED_FACE ( 'NONE', ( #15412 ), #4848, .F. ) ;
#7946 = ORIENTED_EDGE ( 'NONE', *, *, #10260, .F. ) ;
#7947 = SURFACE_STYLE_FILL_AREA ( #8054 ) ;
#7948 = CARTESIAN_POINT ( 'NONE',  ( -90.14671295017259922, 88.16084041142528349, 53.01462269988137876 ) ) ;
#7949 = ORIENTED_EDGE ( 'NONE', *, *, #561, .F. ) ;
#7950 = EDGE_CURVE ( 'NONE', #19868, #7605, #847, .T. ) ;
#7951 = EDGE_CURVE ( 'NONE', #9196, #16304, #1287, .T. ) ;
#7952 = FACE_OUTER_BOUND ( 'NONE', #878, .T. ) ;
#7953 = CARTESIAN_POINT ( 'NONE',  ( 48.54335325434182380, 166.9500029516760833, 274.0152328856624422 ) ) ;
#7954 = DIRECTION ( 'NONE',  ( -0.9999164797902015955, -2.045733645417851287E-15, 0.01292414190464156835 ) ) ;
#7955 = CARTESIAN_POINT ( 'NONE',  ( -36.88402614201490337, 95.89805508694958291, 85.13090641764658528 ) ) ;
#7956 = EDGE_CURVE ( 'NONE', #8451, #10445, #6700, .T. ) ;
#7957 = ORIENTED_EDGE ( 'NONE', *, *, #18375, .T. ) ;
#7958 = CARTESIAN_POINT ( 'NONE',  ( 3.086109933851330151E-14, 20.00000000000000000, 126.0000000000000000 ) ) ;
#7959 = DIRECTION ( 'NONE',  ( -0.5089394657577702707, -0.004781488884709769391, -0.8607890319690654213 ) ) ;
#7960 = CARTESIAN_POINT ( 'NONE',  ( 19.94248262068743571, 183.5029939364791858, 314.4424437290580840 ) ) ;
#7961 = CARTESIAN_POINT ( 'NONE',  ( 50.79373001771442375, 169.4872888238259634, -93.66287481247502456 ) ) ;
#7962 = CARTESIAN_POINT ( 'NONE',  ( -40.65822637310711940, 72.00000000000000000, -84.25167897319539634 ) ) ;
#7963 = B_SPLINE_CURVE_WITH_KNOTS ( 'NONE', 3,
 ( #12166, #1709, #17999, #102, #12399, #6752, #7099, #4067 ),
 .UNSPECIFIED., .F., .F.,
 ( 4, 2, 2, 4 ),
 ( 0.005257893453559862873, 0.006567392922673209558, 0.007876892391786556244, 0.01049589133001325482 ),
 .UNSPECIFIED. ) ;
#7964 = EDGE_CURVE ( 'NONE', #16920, #1331, #12582, .T. ) ;
#7965 = CYLINDRICAL_SURFACE ( 'NONE', #18376, 75.00000000000002842 ) ;
#7966 = CARTESIAN_POINT ( 'NONE',  ( -37.99682623202767928, 170.0000000000000284, 0.4911173923763579863 ) ) ;
#7967 = ORIENTED_EDGE ( 'NONE', *, *, #9347, .T. ) ;
#7968 = DIRECTION ( 'NONE',  ( -0.9909299940865188283, 0.1338359446631173788, 0.01207007604876290420 ) ) ;
#7969 = ORIENTED_EDGE ( 'NONE', *, *, #8240, .T. ) ;
#7970 = ORIENTED_EDGE ( 'NONE', *, *, #5411, .T. ) ;
#7971 = EDGE_CURVE ( 'NONE', #3748, #18558, #1495, .T. ) ;
#7972 = FACE_OUTER_BOUND ( 'NONE', #9979, .T. ) ;
#7973 = ORIENTED_EDGE ( 'NONE', *, *, #11972, .F. ) ;
#7974 = CARTESIAN_POINT ( 'NONE',  ( 75.89440375158403640, 75.05036917497849913, -4.086763113510438750 ) ) ;
#7975 = DIRECTION ( 'NONE',  ( 0.9934404589540162256, 0.1135548637187060589, -0.01346653032743021922 ) ) ;
#7976 = CARTESIAN_POINT ( 'NONE',  ( -106.7514472241618932, 78.38843585434905492, 26.63023763040591163 ) ) ;
#7977 = DIRECTION ( 'NONE',  ( 0.8981428216241984508, 0.000000000000000000, -0.4397038457472520756 ) ) ;
#7978 = EDGE_CURVE ( 'NONE', #21811, #9274, #10339, .T. ) ;
#7979 = ORIENTED_EDGE ( 'NONE', *, *, #5846, .T. ) ;
#7980 = CARTESIAN_POINT ( 'NONE',  ( 10.93157627012523214, 189.7456778768155061, 275.1296412434647323 ) ) ;
#7981 = ORIENTED_EDGE ( 'NONE', *, *, #4914, .T. ) ;
#7982 = DIRECTION ( 'NONE',  ( -3.955169525227119189E-16, -3.753470316973360217E-22, -1.000000000000000000 ) ) ;
#7983 = CARTESIAN_POINT ( 'NONE',  ( -58.12648461715679105, 114.4183207140211209, 172.2192306585357642 ) ) ;
#7984 = CARTESIAN_POINT ( 'NONE',  ( -39.11973256296710133, 107.9236484503692850, 72.42537321791316174 ) ) ;
#7985 = CARTESIAN_POINT ( 'NONE',  ( 91.18542874977053714, 79.95750479416805945, -31.50072335808802038 ) ) ;
#7986 = DIRECTION ( 'NONE',  ( 0.5089394657577702707, 0.004781488884709769391, 0.8607890319690654213 ) ) ;
#7987 = CARTESIAN_POINT ( 'NONE',  ( -41.00000899811524846, 169.5540992312279229, 273.1580453575298293 ) ) ;
#7988 = ORIENTED_EDGE ( 'NONE', *, *, #9485, .F. ) ;
#7989 = FACE_OUTER_BOUND ( 'NONE', #3742, .T. ) ;
#7990 = ADVANCED_FACE ( 'NONE', ( #1608 ), #2289, .F. ) ;
#7991 = ORIENTED_EDGE ( 'NONE', *, *, #19593, .F. ) ;
#7992 = EDGE_CURVE ( 'NONE', #14948, #638, #8474, .T. ) ;
#7993 = VERTEX_POINT ( 'NONE', #10449 ) ;
#7994 = DIRECTION ( 'NONE',  ( 0.7056475024472779189, -0.7085438702141405587, -0.005214045635221192972 ) ) ;
#7995 = CARTESIAN_POINT ( 'NONE',  ( -13.21851778092264240, 183.7781430057642922, 309.6523260561946245 ) ) ;
#7996 = ORIENTED_EDGE ( 'NONE', *, *, #18627, .F. ) ;
#7997 = VECTOR ( 'NONE', #14975, 999.9999999999998863 ) ;
#7998 = EDGE_LOOP ( 'NONE', ( #5278, #9050, #16077 ) ) ;
#7999 = VECTOR ( 'NONE', #417, 1000.000000000000114 ) ;
#8000 = LINE ( 'NONE', #9847, #16251 ) ;
#8001 = ORIENTED_EDGE ( 'NONE', *, *, #15989, .F. ) ;
#8002 = CARTESIAN_POINT ( 'NONE',  ( -41.96503124479402658, 165.8559883853732515, 234.9371320172060678 ) ) ;
#8003 = EDGE_CURVE ( 'NONE', #8988, #1664, #11706, .T. ) ;
#8004 = ADVANCED_FACE ( 'NONE', ( #5367 ), #15983, .T. ) ;
#8005 = PLANE ( 'NONE',  #18812 ) ;
#8006 = ORIENTED_EDGE ( 'NONE', *, *, #11604, .T. ) ;
#8007 = AXIS2_PLACEMENT_3D ( 'NONE', #9782, #16795, #1047 ) ;
#8008 = VERTEX_POINT ( 'NONE', #21117 ) ;
#8009 = DIRECTION ( 'NONE',  ( 0.01292394549866733230, 0.005513023399720419666, 0.9999012842304692006 ) ) ;
#8010 = CARTESIAN_POINT ( 'NONE',  ( 73.74384038452764401, 74.99899999999998101, -0.9531554654672949045 ) ) ;
#8011 = VERTEX_POINT ( 'NONE', #12301 ) ;
#8012 = AXIS2_PLACEMENT_3D ( 'NONE', #14890, #11412, #18424 ) ;
#8013 = CARTESIAN_POINT ( 'NONE',  ( -106.2491592972476155, 77.90302844854605269, -28.48020057081445344 ) ) ;
#8014 = VECTOR ( 'NONE', #5225, 999.9999999999998863 ) ;
#8016 = DIRECTION ( 'NONE',  ( -0.9999164797902015955, -6.965998958219364448E-18, 0.01292414190464157182 ) ) ;
#8015 = DIRECTION ( 'NONE',  ( 7.125109674160258889E-05, -0.9999848031710253382, 0.005512562950849898315 ) ) ;
#8017 = DIRECTION ( 'NONE',  ( 7.125109674403850657E-05, -0.9999848031710253382, 0.005512562950847868688 ) ) ;
#8018 = ORIENTED_EDGE ( 'NONE', *, *, #21294, .F. ) ;
#8019 = ORIENTED_EDGE ( 'NONE', *, *, #8083, .T. ) ;
#8020 = DIRECTION ( 'NONE',  ( 0.01292414190464131335, 0.000000000000000000, 0.9999164797902017066 ) ) ;
#8021 = CARTESIAN_POINT ( 'NONE',  ( 42.33134245603051937, 168.8134312302534283, 56.31375288182659489 ) ) ;
#8022 = ORIENTED_EDGE ( 'NONE', *, *, #14210, .T. ) ;
#8023 = DIRECTION ( 'NONE',  ( -0.01292414190464137060, 0.000000000000000000, -0.9999164797902015955 ) ) ;
#8024 = FACE_OUTER_BOUND ( 'NONE', #13960, .T. ) ;
#8025 = APPLICATION_PROTOCOL_DEFINITION ( 'draft international standard', 'automotive_design', 1998, #13667 ) ;
#8026 = VECTOR ( 'NONE', #15514, 1000.000000000000114 ) ;
#8028 = ORIENTED_EDGE ( 'NONE', *, *, #13450, .F. ) ;
#8027 = ORIENTED_EDGE ( 'NONE', *, *, #15132, .T. ) ;
#8029 = FACE_OUTER_BOUND ( 'NONE', #8591, .T. ) ;
#8030 = ADVANCED_FACE ( 'NONE', ( #2053 ), #453, .F. ) ;
#8031 = DIRECTION ( 'NONE',  ( 0.9999164797902015955, 4.653667080246434899E-16, -0.01292414190464084844 ) ) ;
#8032 = CARTESIAN_POINT ( 'NONE',  ( 48.46580958134982353, 166.9169248112777666, 268.0158251802795917 ) ) ;
#8033 = LINE ( 'NONE', #15067, #18412 ) ;
#8034 = CARTESIAN_POINT ( 'NONE',  ( -51.40218462123966248, 189.4003865961453812, -108.1612621023553658 ) ) ;
#8035 = CARTESIAN_POINT ( 'NONE',  ( -41.56623493000981284, 69.99999999999998579, -82.46967996629571473 ) ) ;
#8036 = DIRECTION ( 'NONE',  ( 1.000000000000000000, -0.000000000000000000, -1.386679829960243376E-14 ) ) ;
#8037 = CARTESIAN_POINT ( 'NONE',  ( 58.06826235119833512, 126.2437860471384568, 43.59380157701544789 ) ) ;
#8038 = ORIENTED_EDGE ( 'NONE', *, *, #7890, .F. ) ;
#8039 = DIRECTION ( 'NONE',  ( 5.440186201345810285E-18, 1.000000000000000000, 1.334940939666369727E-17 ) ) ;
#8040 = ORIENTED_EDGE ( 'NONE', *, *, #10175, .T. ) ;
#8041 = CYLINDRICAL_SURFACE ( 'NONE', #4787, 2.000000000000001332 ) ;
#8042 = LINE ( 'NONE', #20336, #13733 ) ;
#8043 = CARTESIAN_POINT ( 'NONE',  ( 69.43142427201327394, 92.58578643762697880, -85.31868097644085935 ) ) ;
#8044 = DIRECTION ( 'NONE',  ( -0.8981428216242027807, 0.000000000000000000, 0.4397038457472431938 ) ) ;
#8045 = CIRCLE ( 'NONE', #15777, 4.400000000000003908 ) ;
#8046 = CARTESIAN_POINT ( 'NONE',  ( 1.166418432474939088E-15, 20.00000000000000000, 7.999999999999994671 ) ) ;
#8047 = DIRECTION ( 'NONE',  ( 0.01035335185279138807, 0.005513005182356417802, 0.9999312050732649393 ) ) ;
#8048 = CIRCLE ( 'NONE', #18335, 2.499999999999988010 ) ;
#8049 = ORIENTED_EDGE ( 'NONE', *, *, #12333, .T. ) ;
#8050 = DIRECTION ( 'NONE',  ( 0.9909299940865186063, -0.1338359446631179339, -0.01207007604875938098 ) ) ;
#8051 = DIRECTION ( 'NONE',  ( -0.000000000000000000, -1.000000000000000000, -0.000000000000000000 ) ) ;
#8052 = ORIENTED_EDGE ( 'NONE', *, *, #21203, .T. ) ;
#8053 = ORIENTED_EDGE ( 'NONE', *, *, #2526, .F. ) ;
#8054 = FILL_AREA_STYLE ('',( #2790 ) ) ;
#8055 = CARTESIAN_POINT ( 'NONE',  ( -90.17005756999139976, 87.12416931164095502, 51.32274856367679661 ) ) ;
#8056 = VECTOR ( 'NONE', #20300, 1000.000000000000000 ) ;
#8057 = EDGE_LOOP ( 'NONE', ( #6628, #5245, #11730, #1009, #3925, #5113, #18800, #20670 ) ) ;
#8058 = EDGE_CURVE ( 'NONE', #959, #9371, #17350, .T. ) ;
#8059 = AXIS2_PLACEMENT_3D ( 'NONE', #9911, #3468, #17494 ) ;
#8060 = VECTOR ( 'NONE', #20057, 1000.000000000000000 ) ;
#8061 = DIRECTION ( 'NONE',  ( 0.01292394549866738261, 0.005513023399722618428, 0.9999012842304692006 ) ) ;
#8062 = CARTESIAN_POINT ( 'NONE',  ( 13.76115603162017820, 155.5381941787832716, 97.49248393264142010 ) ) ;
#8063 = VERTEX_POINT ( 'NONE', #19615 ) ;
#8064 = EDGE_LOOP ( 'NONE', ( #334, #9113, #11892, #21360, #469, #9337, #2020, #3806, #12631, #4590, #1756, #6081, #6198, #1668, #22255 ) ) ;
#8065 = LINE ( 'NONE', #5790, #3753 ) ;
#8066 = EDGE_CURVE ( 'NONE', #5759, #12590, #20265, .T. ) ;
#8067 = CARTESIAN_POINT ( 'NONE',  ( -88.18706637290659955, 88.71869973106718987, 50.32066939225188662 ) ) ;
#8068 = CARTESIAN_POINT ( 'NONE',  ( 5.149300590115015730, 81.99999999999998579, -98.24794683011701579 ) ) ;
#8069 = DIRECTION ( 'NONE',  ( -7.125109674403838460E-05, 0.9999848031710254492, -0.005512562950847868688 ) ) ;
#8070 = CIRCLE ( 'NONE', #1124, 1.999999999999997780 ) ;
#8071 = ORIENTED_EDGE ( 'NONE', *, *, #6946, .F. ) ;
#8072 = EDGE_CURVE ( 'NONE', #21806, #8178, #12516, .T. ) ;
#8073 = DIRECTION ( 'NONE',  ( -0.9999164797902015955, -6.965998958219364448E-18, 0.01292414190464157182 ) ) ;
#8074 = CARTESIAN_POINT ( 'NONE',  ( -2.824407579846267335, 159.2018743582275988, 324.3940559323744424 ) ) ;
#8075 = CARTESIAN_POINT ( 'NONE',  ( 17.56092566177725800, 186.7283010723397751, 319.0062387086613285 ) ) ;
#8076 = DIRECTION ( 'NONE',  ( 0.000000000000000000, 0.000000000000000000, -1.000000000000000000 ) ) ;
#8077 = DIRECTION ( 'NONE',  ( -0.01292394549866742078, -0.005513023399720777019, -0.9999012842304693116 ) ) ;
#8078 = ORIENTED_EDGE ( 'NONE', *, *, #2550, .F. ) ;
#8079 = SHAPE_REPRESENTATION_RELATIONSHIP ( 'NONE' , 'NONE' ,  #21889, #5233 ) ;
#8080 = VECTOR ( 'NONE', #13632, 1000.000000000000000 ) ;
#8081 = PRODUCT ( 'Socket Head Cap Screw', 'Socket Head Cap Screw', '', ( #18380 ) ) ;
#8082 = CIRCLE ( 'NONE', #1115, 87.00000000000001421 ) ;
#8083 = EDGE_CURVE ( 'NONE', #6883, #11658, #19506, .T. ) ;
#8084 = DIRECTION ( 'NONE',  ( 0.01292414190463827932, 0.000000000000000000, 0.9999164797902018176 ) ) ;
#8085 = CARTESIAN_POINT ( 'NONE',  ( 3.872354045398203937, 166.6517708494369856, 299.5967279023338392 ) ) ;
#8086 = EDGE_CURVE ( 'NONE', #12626, #5578, #22030, .T. ) ;
#8087 = ORIENTED_EDGE ( 'NONE', *, *, #5102, .T. ) ;
#8088 = AXIS2_PLACEMENT_3D ( 'NONE', #5847, #11031, #21682 ) ;
#8089 = CARTESIAN_POINT ( 'NONE',  ( -12.66072403271054903, 184.5155800142387363, 278.5994379001652987 ) ) ;
#8090 = ORIENTED_EDGE ( 'NONE', *, *, #17950, .T. ) ;
#8091 = CARTESIAN_POINT ( 'NONE',  ( 48.26619062019285167, 111.5068095596782314, -44.80573832231973341 ) ) ;
#8092 = CARTESIAN_POINT ( 'NONE',  ( 68.71681667565954399, 69.99999999999998579, -85.89527988174788220 ) ) ;
#8093 = ADVANCED_FACE ( 'NONE', ( #16091 ), #3885, .F. ) ;
#8094 = CIRCLE ( 'NONE', #20920, 8.520833333333289517 ) ;
#8095 = VERTEX_POINT ( 'NONE', #3983 ) ;
#8096 =( NAMED_UNIT ( * ) PLANE_ANGLE_UNIT ( ) SI_UNIT ( $, .RADIAN. ) );
#8097 = PLANE ( 'NONE',  #15883 ) ;
#8098 = AXIS2_PLACEMENT_3D ( 'NONE', #7367, #5184, #21375 ) ;
#8099 = EDGE_CURVE ( 'NONE', #3163, #9820, #7219, .T. ) ;
#8100 = CARTESIAN_POINT ( 'NONE',  ( 105.6376945813395025, 78.65441476617404248, -30.67074184297056405 ) ) ;
#8101 = CIRCLE ( 'NONE', #21631, 7.499999999999991118 ) ;
#8102 = LINE ( 'NONE', #5793, #10023 ) ;
#8103 = EDGE_CURVE ( 'NONE', #11316, #164, #17700, .T. ) ;
#8104 = VECTOR ( 'NONE', #10282, 1000.000000000000114 ) ;
#8105 =( BOUNDED_SURFACE ( )  B_SPLINE_SURFACE ( 3, 3, ( 
 ( #7535, #8813, #1713, #1601 ),
 ( #19040, #3306, #10330, #2243 ),
 ( #5786, #14455, #8590, #9363 ),
 ( #8692, #22574, #12821, #11321 ) ),
 .UNSPECIFIED., .F., .F., .T. ) 
 B_SPLINE_SURFACE_WITH_KNOTS ( ( 4, 4 ),
 ( 4, 4 ),
 ( 0.000000000000000000, 1.000000000000000000 ),
 ( 0.000000000000000000, 1.000000000000000000 ),
 .UNSPECIFIED. ) 
 GEOMETRIC_REPRESENTATION_ITEM ( )  RATIONAL_B_SPLINE_SURFACE ( (
 ( 1.000000000000000000, 0.5185431720251972854, 0.5185431720251972854, 1.000000000000000000),
 ( 0.8047378541243652705, 0.4172913195263988628, 0.4172913195263988628, 0.8047378541243652705),
 ( 0.8047378541243652705, 0.4172913195263988628, 0.4172913195263988628, 0.8047378541243652705),
 ( 1.000000000000000000, 0.5185431720251972854, 0.5185431720251972854, 1.000000000000000000) ) ) 
 REPRESENTATION_ITEM ( '' )  SURFACE ( )  );
#8106 = CARTESIAN_POINT ( 'NONE',  ( 21.22526757802852515, 185.7451911998024343, 276.2648941004949847 ) ) ;
#8107 = FACE_OUTER_BOUND ( 'NONE', #17152, .T. ) ;
#8108 = CARTESIAN_POINT ( 'NONE',  ( 41.75993663531772171, 94.85495732055906615, 83.18988100811523623 ) ) ;
#8109 = DIRECTION ( 'NONE',  ( -7.125109674025824596E-05, 0.9999848031710253382, -0.005512562950849464634 ) ) ;
#8110 = DIRECTION ( 'NONE',  ( 0.9934404589540163366, 0.1135548637187051429, -0.01346653032743023309 ) ) ;
#8111 = EDGE_CURVE ( 'NONE', #21136, #18552, #7069, .T. ) ;
#8113 = CARTESIAN_POINT ( 'NONE',  ( 92.11140453220075131, 79.82915613195545745, -31.20677464679435076 ) ) ;
#8112 = B_SPLINE_CURVE_WITH_KNOTS ( 'NONE', 3,
 ( #18559, #16844, #20721, #20485, #15469, #13621 ),
 .UNSPECIFIED., .F., .F.,
 ( 4, 2, 4 ),
 ( 2.403703357979454770E-17, 0.0009937831915592871320, 0.001987566383118549978 ),
 .UNSPECIFIED. ) ;
#8114 = CIRCLE ( 'NONE', #9951, 1.999999999999997780 ) ;
#8115 = DIRECTION ( 'NONE',  ( -0.01292394549866728373, -0.005513023399720296501, -0.9999012842304693116 ) ) ;
#8116 = ORIENTED_EDGE ( 'NONE', *, *, #18153, .T. ) ;
#8117 = FACE_OUTER_BOUND ( 'NONE', #18940, .T. ) ;
#8118 = ORIENTED_EDGE ( 'NONE', *, *, #18410, .T. ) ;
#8119 = CARTESIAN_POINT ( 'NONE',  ( -53.12424548001075664, 118.8900173874207837, 162.2800983528087215 ) ) ;
#8120 = CARTESIAN_POINT ( 'NONE',  ( -13.32411518825262853, 183.5971624586300948, 309.7568532065889713 ) ) ;
#8121 = ORIENTED_EDGE ( 'NONE', *, *, #19527, .T. ) ;
#8122 = ADVANCED_FACE ( 'NONE', ( #7107 ), #16212, .T. ) ;
#8123 = ORIENTED_EDGE ( 'NONE', *, *, #7101, .F. ) ;
#8124 = AXIS2_PLACEMENT_3D ( 'NONE', #2121, #291, #13966 ) ;
#8125 = ADVANCED_FACE ( 'NONE', ( #9283 ), #2304, .F. ) ;
#8126 =( GEOMETRIC_REPRESENTATION_CONTEXT ( 3 ) GLOBAL_UNCERTAINTY_ASSIGNED_CONTEXT ( ( #8743 ) ) GLOBAL_UNIT_ASSIGNED_CONTEXT ( ( #3324, #5034, #10228 ) ) REPRESENTATION_CONTEXT ( 'NONE', 'WORKASPACE' ) );
#8127 = VECTOR ( 'NONE', #9812, 1000.000000000000227 ) ;
#8128 = CARTESIAN_POINT ( 'NONE',  ( -66.73173682738223533, 70.03297899285537653, 87.44705638319801722 ) ) ;
#8129 = AXIS2_PLACEMENT_3D ( 'NONE', #2109, #9100, #12578 ) ;
#8130 = CARTESIAN_POINT ( 'NONE',  ( -51.07890516687701421, 106.8060942374655156, 71.59941146007480484 ) ) ;
#8131 = DIRECTION ( 'NONE',  ( 7.125109674161246868E-05, -0.9999848031710252272, 0.005512562950850154186 ) ) ;
#8132 = EDGE_CURVE ( 'NONE', #7137, #12590, #21881, .T. ) ;
#8133 = CARTESIAN_POINT ( 'NONE',  ( 65.33690683320658366, 190.1463355405889786, 25.64579400984300150 ) ) ;
#8134 = VECTOR ( 'NONE', #2958, 999.9999999999998863 ) ;
#8135 = ORIENTED_EDGE ( 'NONE', *, *, #3872, .F. ) ;
#8136 = CIRCLE ( 'NONE', #12910, 6.000000000000000888 ) ;
#8137 = CARTESIAN_POINT ( 'NONE',  ( 54.52327687265660927, 1.999999999999998224, -111.3697098814019313 ) ) ;
#8138 = LINE ( 'NONE', #20302, #21680 ) ;
#8139 =( NAMED_UNIT ( * ) PLANE_ANGLE_UNIT ( ) SI_UNIT ( $, .RADIAN. ) );
#8141 = DIRECTION ( 'NONE',  ( 0.01292394549866743465, 0.005513023399721021615, 0.9999012842304692006 ) ) ;
#8140 = DIRECTION ( 'NONE',  ( 0.000000000000000000, 0.000000000000000000, -1.000000000000000000 ) ) ;
#8142 = CARTESIAN_POINT ( 'NONE',  ( -8.312614011469616315, 81.99999999999998579, -95.45924547291811280 ) ) ;
#8143 = EDGE_LOOP ( 'NONE', ( #20766, #1644 ) ) ;
#8144 = DIRECTION ( 'NONE',  ( -0.9999164797902015955, -2.001050586450181282E-22, 0.01292414190463992731 ) ) ;
#8145 = DIRECTION ( 'NONE',  ( 0.01292414190464131335, 1.902755938799530239E-22, 0.9999164797902015955 ) ) ;
#8146 = VECTOR ( 'NONE', #10825, 999.9999999999998863 ) ;
#8147 = LINE ( 'NONE', #6642, #10986 ) ;
#8148 = ADVANCED_FACE ( 'NONE', ( #4556 ), #2843, .F. ) ;
#8149 = ORIENTED_EDGE ( 'NONE', *, *, #4727, .F. ) ;
#8150 = VECTOR ( 'NONE', #6714, 1000.000000000000114 ) ;
#8151 = CYLINDRICAL_SURFACE ( 'NONE', #8402, 95.00000000000004263 ) ;
#8152 = AXIS2_PLACEMENT_3D ( 'NONE', #22570, #10664, #14130 ) ;
#8153 = AXIS2_PLACEMENT_3D ( 'NONE', #6072, #2514, #918 ) ;
#8154 = LINE ( 'NONE', #15183, #18078 ) ;
#8156 = ORIENTED_EDGE ( 'NONE', *, *, #17287, .F. ) ;
#8155 = VERTEX_POINT ( 'NONE', #6177 ) ;
#8157 = CARTESIAN_POINT ( 'NONE',  ( -52.88443356760686953, 109.6548370181895962, -43.48813313179322648 ) ) ;
#8158 = DIRECTION ( 'NONE',  ( -0.01292394549866731669, -0.005513023399720593139, -0.9999012842304692006 ) ) ;
#8159 = CIRCLE ( 'NONE', #14044, 75.00000000000002842 ) ;
#8160 = CARTESIAN_POINT ( 'NONE',  ( -1.421655609510531049, 105.0000000000000000, -109.9908127769221977 ) ) ;
#8161 = CARTESIAN_POINT ( 'NONE',  ( 3.866440703273599677, 81.64368954560637803, -81.75340644824424885 ) ) ;
#8162 = DIRECTION ( 'NONE',  ( -5.440186201345738641E-18, -1.000000000000000000, -1.334940939666364181E-17 ) ) ;
#8163 = CARTESIAN_POINT ( 'NONE',  ( 49.40018710923111911, 94.98683777375578074, -46.72950894661879317 ) ) ;
#8164 = ORIENTED_EDGE ( 'NONE', *, *, #15708, .T. ) ;
#8165 = CARTESIAN_POINT ( 'NONE',  ( 37.28121903589197217, 92.86731729164014837, -84.62157808539689086 ) ) ;
#8166 = DIRECTION ( 'NONE',  ( -0.000000000000000000, -1.000000000000000000, -0.000000000000000000 ) ) ;
#8167 = ORIENTED_EDGE ( 'NONE', *, *, #13386, .F. ) ;
#8168 = DIRECTION ( 'NONE',  ( 0.3834992599886432041, -0.005063754594578209756, -0.9235273011544211652 ) ) ;
#8169 = LINE ( 'NONE', #10121, #2726 ) ;
#8170 = CARTESIAN_POINT ( 'NONE',  ( 106.2052848363078539, 71.73256685213068806, 28.64329287727201034 ) ) ;
#8171 = CARTESIAN_POINT ( 'NONE',  ( -4.720905924553975730, 165.6695212782702811, 299.7132133896669188 ) ) ;
#8172 = AXIS2_PLACEMENT_3D ( 'NONE', #8248, #20513, #17317 ) ;
#8173 = AXIS2_PLACEMENT_3D ( 'NONE', #4028, #11281, #16472 ) ;
#8174 = ORIENTED_EDGE ( 'NONE', *, *, #6023, .T. ) ;
#8175 = DIRECTION ( 'NONE',  ( 7.125109674160258889E-05, -0.9999848031710253382, 0.005512562950849898315 ) ) ;
#8176 = DIRECTION ( 'NONE',  ( -0.01292414190464132896, 0.000000000000000000, -0.9999164797902015955 ) ) ;
#8177 = DIRECTION ( 'NONE',  ( 0.9999164797902017066, 2.001050586450178931E-22, -0.01292414190464131508 ) ) ;
#8178 = VERTEX_POINT ( 'NONE', #4218 ) ;
#8179 = CARTESIAN_POINT ( 'NONE',  ( 47.57075801145018801, 94.99786382055530964, -44.70572651227904970 ) ) ;
#8180 = EDGE_CURVE ( 'NONE', #22352, #20855, #21001, .T. ) ;
#8181 = VECTOR ( 'NONE', #10897, 1000.000000000000000 ) ;
#8182 = DIRECTION ( 'NONE',  ( 0.7944560844389300103, 0.000000000000000000, 0.6073216033519338586 ) ) ;
#8183 = ADVANCED_FACE ( 'NONE', ( #9510 ), #113, .F. ) ;
#8184 = ORIENTED_EDGE ( 'NONE', *, *, #14504, .T. ) ;
#8185 = DIRECTION ( 'NONE',  ( -0.01292394549866738608, -0.005513023399720698957, -0.9999012842304692006 ) ) ;
#8186 = CARTESIAN_POINT ( 'NONE',  ( -89.97337599888878401, 88.77373198860428261, 52.43004476888089727 ) ) ;
#8188 = FACE_OUTER_BOUND ( 'NONE', #7632, .T. ) ;
#8187 = CIRCLE ( 'NONE', #20632, 10.00000000000000888 ) ;
#8190 = ORIENTED_EDGE ( 'NONE', *, *, #10736, .F. ) ;
#8189 = VERTEX_POINT ( 'NONE', #14707 ) ;
#8191 = TOROIDAL_SURFACE ( 'NONE', #3789, 8.000000000000014211, 2.000000000000000000 ) ;
#8192 = CYLINDRICAL_SURFACE ( 'NONE', #7761, 120.0000000000000000 ) ;
#8193 = CARTESIAN_POINT ( 'NONE',  ( -79.92740525950245001, 55.00000000000000000, 6.133505399301367511 ) ) ;
#8194 = CARTESIAN_POINT ( 'NONE',  ( -35.95309506732429128, 93.50464841319750064, -82.03286182426641915 ) ) ;
#8195 = CARTESIAN_POINT ( 'NONE',  ( 146.4999999999998863, 1.999999999999998224, -8.000000000002026823 ) ) ;
#8196 = CARTESIAN_POINT ( 'NONE',  ( -46.67741832313596717, 141.4150907639732679, 257.3849938494272465 ) ) ;
#8197 = CARTESIAN_POINT ( 'NONE',  ( -51.17277943929727968, 189.4982449580671471, -90.41261591246242801 ) ) ;
#8198 = ORIENTED_EDGE ( 'NONE', *, *, #11263, .T. ) ;
#8199 = EDGE_LOOP ( 'NONE', ( #17123, #7967, #22303 ) ) ;
#8200 = DIRECTION ( 'NONE',  ( -0.009985269297343229641, -0.6348858185549676181, -0.7725414498878673264 ) ) ;
#8201 = LINE ( 'NONE', #6479, #21757 ) ;
#8202 = CIRCLE ( 'NONE', #11133, 112.5000000000000142 ) ;
#8203 = CARTESIAN_POINT ( 'NONE',  ( 15.62064282387073710, 186.1419012809306253, 320.4776025279708733 ) ) ;
#8204 = CARTESIAN_POINT ( 'NONE',  ( 58.84369908111836622, 126.5745674511216947, 103.5878786308435906 ) ) ;
#8205 = VERTEX_POINT ( 'NONE', #11244 ) ;
#8206 = DIRECTION ( 'NONE',  ( 7.125109674364536131E-05, -0.9999848031710253382, 0.005512562950849705760 ) ) ;
#8207 = AXIS2_PLACEMENT_3D ( 'NONE', #1447, #10065, #4976 ) ;
#8208 = AXIS2_PLACEMENT_3D ( 'NONE', #10735, #1774, #5085 ) ;
#8209 = EDGE_CURVE ( 'NONE', #8963, #1725, #7667, .T. ) ;
#8210 = CARTESIAN_POINT ( 'NONE',  ( 162.0000000000000000, 18.00000000000000355, -2.262479907570351121E-12 ) ) ;
#8211 = LINE ( 'NONE', #11996, #16595 ) ;
#8212 = EDGE_LOOP ( 'NONE', ( #20133, #5003, #1763, #16356 ) ) ;
#8213 = CARTESIAN_POINT ( 'NONE',  ( -12.43529986855201486, 186.4710608878919516, 276.5579441034727779 ) ) ;
#8214 = ORIENTED_EDGE ( 'NONE', *, *, #14431, .T. ) ;
#8215 = EDGE_CURVE ( 'NONE', #5625, #20105, #6065, .T. ) ;
#8216 = EDGE_LOOP ( 'NONE', ( #10146, #15839, #8482, #12667, #15850, #13501, #8833, #7081 ) ) ;
#8217 = CARTESIAN_POINT ( 'NONE',  ( -88.73519446327063065, 70.71303863658374667, 62.85397390640905257 ) ) ;
#8218 = AXIS2_PLACEMENT_3D ( 'NONE', #16129, #4023, #7488 ) ;
#8219 = ORIENTED_EDGE ( 'NONE', *, *, #880, .T. ) ;
#8220 = CARTESIAN_POINT ( 'NONE',  ( -44.54866185121051103, 164.1908348453399640, 35.20998652991943345 ) ) ;
#8221 = FACE_OUTER_BOUND ( 'NONE', #5195, .T. ) ;
#8222 = CIRCLE ( 'NONE', #4175, 126.0000000000000000 ) ;
#8223 = DIRECTION ( 'NONE',  ( 0.9999164797902017066, 6.965998958219365988E-18, -0.01292414190464157356 ) ) ;
#8224 = ADVANCED_FACE ( 'NONE', ( #1014 ), #8005, .T. ) ;
#8225 = DIRECTION ( 'NONE',  ( 0.01292394549866738955, 0.005513023399720468239, 0.9999012842304693116 ) ) ;
#8226 = CARTESIAN_POINT ( 'NONE',  ( 6.523188911928189171, 81.98100004360546222, -85.22790637956201465 ) ) ;
#8227 = LINE ( 'NONE', #6722, #10037 ) ;
#8228 = FACE_OUTER_BOUND ( 'NONE', #9121, .T. ) ;
#8229 = ADVANCED_FACE ( 'NONE', ( #18355 ), #9214, .F. ) ;
#8230 = DIRECTION ( 'NONE',  ( 0.01292414190464131335, 1.902755938799531179E-22, 0.9999164797902017066 ) ) ;
#8231 = DIRECTION ( 'NONE',  ( -0.006350819331212801712, 0.8709385446395347952, -0.4913509118287984201 ) ) ;
#8232 = VECTOR ( 'NONE', #919, 1000.000000000000000 ) ;
#8233 = EDGE_LOOP ( 'NONE', ( #4665, #19244, #4615, #20842 ) ) ;
#8234 = DIRECTION ( 'NONE',  ( 0.003413786507415475339, -0.9644842718275420390, 0.2641182225045781706 ) ) ;
#8235 = CARTESIAN_POINT ( 'NONE',  ( 52.34460878051607580, 84.99999999999997158, 26.32568957529409204 ) ) ;
#8236 = VERTEX_POINT ( 'NONE', #5821 ) ;
#8237 = DIRECTION ( 'NONE',  ( 0.9999164797902015955, 6.965998958219364448E-18, -0.01292414190464157182 ) ) ;
#8238 = EDGE_CURVE ( 'NONE', #10247, #14770, #16173, .T. ) ;
#8239 = VERTEX_POINT ( 'NONE', #21998 ) ;
#8240 = EDGE_CURVE ( 'NONE', #1849, #2415, #2202, .T. ) ;
#8241 = AXIS2_PLACEMENT_3D ( 'NONE', #15923, #19332, #2002 ) ;
#8242 = EDGE_CURVE ( 'NONE', #4784, #3676, #4103, .T. ) ;
#8243 = CARTESIAN_POINT ( 'NONE',  ( 106.9749367633763910, 78.91761970611439381, 25.61958048976759983 ) ) ;
#8244 =( BOUNDED_SURFACE ( )  B_SPLINE_SURFACE ( 3, 2, ( 
 ( #5111, #2952, #17439 ),
 ( #4771, #10422, #8670 ),
 ( #22226, #6518, #17196 ),
 ( #8450, #10090, #10194 ),
 ( #12031, #6629, #17102 ),
 ( #20748, #10307, #1364 ),
 ( #8340, #13652, #1472 ),
 ( #22449, #6741, #13765 ),
 ( #5002, #19018, #3280 ),
 ( #20970, #12723, #5228 ),
 ( #1921, #12382, #19363 ),
 ( #5689, #5454, #10531 ),
 ( #19689, #17672, #12268 ),
 ( #13982, #16184, #15719 ),
 ( #8908, #7080, #3958 ),
 ( #12610, #2133, #19255 ),
 ( #10981, #2031, #21090 ),
 ( #9132, #5579, #15957 ) ),
 .UNSPECIFIED., .F., .F., .T. ) 
 B_SPLINE_SURFACE_WITH_KNOTS ( ( 4, 2, 2, 2, 2, 2, 2, 2, 4 ),
 ( 3, 3 ),
 ( 0.08392082777195179755, 0.08669808355441036007, 0.08808671144563964828, 0.08878102539125429238, 0.08912818236406161443, 0.08930176085046526158, 0.08934515547206617336, 0.08938855009366708515, 0.08947533933686892260 ),
 ( 0.000000000000000000, 1.000000000000000000 ),
 .UNSPECIFIED. ) 
 GEOMETRIC_REPRESENTATION_ITEM ( )  RATIONAL_B_SPLINE_SURFACE ( (
 ( 1.000000000000000000, 0.8227386401547606143, 1.000000000000000000),
 ( 1.000000000000000000, 0.8263415838640109090, 1.000000000000000000),
 ( 1.000000000000000000, 0.8288608359785593072, 1.000000000000000000),
 ( 1.000000000000000000, 0.8282189721136420379, 1.000000000000000000),
 ( 1.000000000000000000, 0.8271574078587653478, 1.000000000000000000),
 ( 1.000000000000000000, 0.8239197622725578096, 1.000000000000000000),
 ( 1.000000000000000000, 0.8225730560359920673, 1.000000000000000000),
 ( 1.000000000000000000, 0.8201245374487728945, 1.000000000000000000),
 ( 1.000000000000000000, 0.8192370252838325762, 1.000000000000000000),
 ( 1.000000000000000000, 0.8177961922896359592, 1.000000000000000000),
 ( 1.000000000000000000, 0.8172976608657051001, 1.000000000000000000),
 ( 1.000000000000000000, 0.8166514735311385387, 1.000000000000000000),
 ( 1.000000000000000000, 0.8167936669053370569, 1.000000000000000000),
 ( 1.000000000000000000, 0.8168953424619973536, 1.000000000000000000),
 ( 1.000000000000000000, 0.8169461963296643647, 1.000000000000000000),
 ( 1.000000000000000000, 0.8170988061662717294, 1.000000000000000000),
 ( 1.000000000000000000, 0.8172006103767126550, 1.000000000000000000),
 ( 1.000000000000000000, 0.8173024788409366526, 1.000000000000000000) ) ) 
 REPRESENTATION_ITEM ( '' )  SURFACE ( )  );
#8245 = AXIS2_PLACEMENT_3D ( 'NONE', #11857, #18619, #14973 ) ;
#8246 = CARTESIAN_POINT ( 'NONE',  ( -2.679299502224010254, 326.9817443121281713, 308.2885977099632555 ) ) ;
#8247 = EDGE_CURVE ( 'NONE', #13913, #5652, #11585, .T. ) ;
#8248 = CARTESIAN_POINT ( 'NONE',  ( -154.0000000000000000, 1.999999999999998224, -53.76161406891256433 ) ) ;
#8249 = LINE ( 'NONE', #11934, #5818 ) ;
#8250 = EDGE_LOOP ( 'NONE', ( #12062, #19828 ) ) ;
#8251 = AXIS2_PLACEMENT_3D ( 'NONE', #1488, #1382, #17016 ) ;
#8252 = EDGE_CURVE ( 'NONE', #4037, #9196, #11131, .T. ) ;
#8253 = CARTESIAN_POINT ( 'NONE',  ( -66.06691928577359363, 94.02752048664900997, -82.12548041065298321 ) ) ;
#8254 = DIRECTION ( 'NONE',  ( -0.000000000000000000, -1.000000000000000000, -0.000000000000000000 ) ) ;
#8255 = DIRECTION ( 'NONE',  ( 0.9999164797902017066, 2.001050586450178931E-22, -0.01292414190464131508 ) ) ;
#8256 = ORIENTED_EDGE ( 'NONE', *, *, #13178, .F. ) ;
#8257 = DIRECTION ( 'NONE',  ( 0.000000000000000000, 1.000000000000000000, 0.000000000000000000 ) ) ;
#8258 = CARTESIAN_POINT ( 'NONE',  ( 65.88241411543798165, 104.3814432989690602, 67.85066342192635602 ) ) ;
#8259 = B_SPLINE_CURVE_WITH_KNOTS ( 'NONE', 3,
 ( #9468, #11213, #20132, #4405 ),
 .UNSPECIFIED., .F., .F.,
 ( 4, 4 ),
 ( 0.000000000000000000, 0.0001170083130068365703 ),
 .UNSPECIFIED. ) ;
#8260 = FACE_OUTER_BOUND ( 'NONE', #8669, .T. ) ;
#8261 = CARTESIAN_POINT ( 'NONE',  ( -24.08933336292039229, 324.5818098845193731, 320.3078767544336642 ) ) ;
#8262 = EDGE_CURVE ( 'NONE', #15798, #9516, #2404, .T. ) ;
#8263 = CARTESIAN_POINT ( 'NONE',  ( 1.417778366939166146, 45.00000000000000000, 109.6908378329851246 ) ) ;
#8264 = DIRECTION ( 'NONE',  ( 0.01292394549866738261, 0.005513023399722618428, 0.9999012842304692006 ) ) ;
#8265 = APPLICATION_PROTOCOL_DEFINITION ( 'draft international standard', 'automotive_design', 1998, #21842 ) ;
#8266 = ORIENTED_EDGE ( 'NONE', *, *, #12387, .F. ) ;
#8267 = CARTESIAN_POINT ( 'NONE',  ( -50.64859668917933533, 109.1804550457673884, -45.80181734348686717 ) ) ;
#8268 = DIRECTION ( 'NONE',  ( -7.125109674161230605E-05, 0.9999848031710253382, -0.005512562950850140309 ) ) ;
#8269 = CARTESIAN_POINT ( 'NONE',  ( 0.000000000000000000, 25.00000000000000000, 0.000000000000000000 ) ) ;
#8270 = DIRECTION ( 'NONE',  ( -0.01292394549866739996, -0.005513023399721131770, -0.9999012842304692006 ) ) ;
#8271 = MECHANICAL_DESIGN_GEOMETRIC_PRESENTATION_REPRESENTATION (  '', ( #1309 ), #21459 ) ;
#8272 = LINE ( 'NONE', #14961, #6463 ) ;
#8273 = DIRECTION ( 'NONE',  ( 1.000000000000000000, -0.000000000000000000, -1.386679829960243376E-14 ) ) ;
#8274 = ORIENTED_EDGE ( 'NONE', *, *, #1910, .F. ) ;
#8275 = ADVANCED_FACE ( 'NONE', ( #678 ), #17631, .T. ) ;
#8276 = FACE_OUTER_BOUND ( 'NONE', #8644, .T. ) ;
#8277 = EDGE_LOOP ( 'NONE', ( #9144, #13542, #14556, #11965 ) ) ;
#8278 = CARTESIAN_POINT ( 'NONE',  ( -154.0000000000000000, 0.000000000000000000, -53.76161406891256433 ) ) ;
#8279 = CARTESIAN_POINT ( 'NONE',  ( -16.82962413914983912, 177.4987173824078468, 90.66609475777795524 ) ) ;
#8280 = DIRECTION ( 'NONE',  ( -0.01292414190463830014, 0.000000000000000000, -0.9999164797902017066 ) ) ;
#8281 = PLANE ( 'NONE',  #22343 ) ;
#8282 = CARTESIAN_POINT ( 'NONE',  ( 162.0000000000000000, 18.00000000000000355, 2.222801351277976832E-12 ) ) ;
#8283 = CARTESIAN_POINT ( 'NONE',  ( 12.82628922073134170, 190.6145596806321407, 307.8497150165550238 ) ) ;
#8284 = ORIENTED_EDGE ( 'NONE', *, *, #20592, .T. ) ;
#8285 = CARTESIAN_POINT ( 'NONE',  ( 6.808509919968707358, 82.00000000000000000, -94.26135563083259683 ) ) ;
#8286 = EDGE_CURVE ( 'NONE', #17192, #14240, #10100, .T. ) ;
#8287 = FACE_OUTER_BOUND ( 'NONE', #1899, .T. ) ;
#8288 = EDGE_LOOP ( 'NONE', ( #16322, #12346, #14812, #1437 ) ) ;
#8289 = CIRCLE ( 'NONE', #16743, 3.999999999999995559 ) ;
#8290 = PLANE ( 'NONE',  #8736 ) ;
#8291 = CARTESIAN_POINT ( 'NONE',  ( -88.16466383535862406, 88.38054089998362883, 52.81015645075888898 ) ) ;
#8292 = VERTEX_POINT ( 'NONE', #22562 ) ;
#8293 = CARTESIAN_POINT ( 'NONE',  ( -1.079165849037536207, 44.99899999999999523, -83.49302606248184588 ) ) ;
#8294 = LINE ( 'NONE', #9575, #1556 ) ;
#8295 = DIRECTION ( 'NONE',  ( 0.9999164797902017066, 0.000000000000000000, -0.01292414190464177826 ) ) ;
#8296 = FACE_OUTER_BOUND ( 'NONE', #18258, .T. ) ;
#8297 = FACE_OUTER_BOUND ( 'NONE', #15098, .T. ) ;
#8298 = CARTESIAN_POINT ( 'NONE',  ( -55.33804461215960657, 114.2193244133317904, 167.6379947637574617 ) ) ;
#8299 = EDGE_CURVE ( 'NONE', #6442, #5484, #17266, .T. ) ;
#8300 = ORIENTED_EDGE ( 'NONE', *, *, #22227, .F. ) ;
#8301 = EDGE_CURVE ( 'NONE', #19631, #9627, #6611, .T. ) ;
#8302 = FACE_OUTER_BOUND ( 'NONE', #7724, .T. ) ;
#8303 = LINE ( 'NONE', #15336, #22135 ) ;
#8304 = CARTESIAN_POINT ( 'NONE',  ( -35.42010074854528767, 108.0982075334647163, 199.8475074598744357 ) ) ;
#8305 = CARTESIAN_POINT ( 'NONE',  ( 12.16442896649338223, 187.7168230983759543, 322.9757373289252200 ) ) ;
#8306 = CARTESIAN_POINT ( 'NONE',  ( -10.07101741848119936, 146.4908573800363456, 278.3054745090071833 ) ) ;
#8307 = DIRECTION ( 'NONE',  ( 7.125109674364534776E-05, -0.9999848031710252272, 0.005512562950849704893 ) ) ;
#8308 = CARTESIAN_POINT ( 'NONE',  ( 13.42006642051110177, 160.8124487847600221, 323.5078865155649055 ) ) ;
#8309 = ORIENTED_EDGE ( 'NONE', *, *, #12603, .T. ) ;
#8310 = CARTESIAN_POINT ( 'NONE',  ( -9.043880562332304862, 187.2595245844938177, 277.6087870137185973 ) ) ;
#8311 = ORIENTED_EDGE ( 'NONE', *, *, #742, .F. ) ;
#8312 = VERTEX_POINT ( 'NONE', #15852 ) ;
#8313 = CARTESIAN_POINT ( 'NONE',  ( -1.079165849037536207, 69.99999999999998579, -83.49302606248184588 ) ) ;
#8314 = ORIENTED_EDGE ( 'NONE', *, *, #13656, .T. ) ;
#8315 = SURFACE_STYLE_USAGE ( .BOTH. , #20822 ) ;
#8316 = CARTESIAN_POINT ( 'NONE',  ( -7.475646132950418021, 81.19615242270661781, -81.73701953211944726 ) ) ;
#8317 = CARTESIAN_POINT ( 'NONE',  ( 80.88825763458693530, 75.20315502959410026, 5.165049547085412307 ) ) ;
#8318 = DIRECTION ( 'NONE',  ( 0.000000000000000000, 0.000000000000000000, 1.000000000000000000 ) ) ;
#8319 = DIRECTION ( 'NONE',  ( 0.000000000000000000, 0.000000000000000000, 1.000000000000000000 ) ) ;
#8320 = CARTESIAN_POINT ( 'NONE',  ( -146.5000000000000000, 18.00000000000000355, -9.999999999999982236 ) ) ;
#8321 = DIRECTION ( 'NONE',  ( 0.000000000000000000, -1.000000000000000000, 0.000000000000000000 ) ) ;
#8322 = CARTESIAN_POINT ( 'NONE',  ( 41.14038128610372524, 95.59192558790229555, 83.85389257729781320 ) ) ;
#8323 = FACE_OUTER_BOUND ( 'NONE', #9672, .T. ) ;
#8324 = CARTESIAN_POINT ( 'NONE',  ( 4.177359159166812219, 166.7818782016704802, 323.1943982101736879 ) ) ;
#8325 = CARTESIAN_POINT ( 'NONE',  ( -2.067862704742604141, 69.99999999999998579, -159.9866367664322979 ) ) ;
#8326 = CARTESIAN_POINT ( 'NONE',  ( -40.19002855417061681, 106.9581283947334924, 71.59385384405536001 ) ) ;
#8327 = VECTOR ( 'NONE', #7671, 1000.000000000000114 ) ;
#8328 = ORIENTED_EDGE ( 'NONE', *, *, #10385, .F. ) ;
#8329 = CARTESIAN_POINT ( 'NONE',  ( -8.301606475021044318, 185.5510420931183546, 308.0304484427728084 ) ) ;
#8330 = ORIENTED_EDGE ( 'NONE', *, *, #20378, .T. ) ;
#8331 = DIRECTION ( 'NONE',  ( 0.000000000000000000, 0.000000000000000000, -1.000000000000000000 ) ) ;
#8332 = VERTEX_POINT ( 'NONE', #11939 ) ;
#8333 = EDGE_CURVE ( 'NONE', #12220, #2857, #3727, .T. ) ;
#8334 = DIRECTION ( 'NONE',  ( 0.9999164797902017066, 6.965998958219365988E-18, -0.01292414190464157356 ) ) ;
#8335 = DIRECTION ( 'NONE',  ( 5.440186201345738641E-18, 1.000000000000000000, 1.334940939666364181E-17 ) ) ;
#8337 = AXIS2_PLACEMENT_3D ( 'NONE', #13569, #20782, #4811 ) ;
#8336 = DIRECTION ( 'NONE',  ( 0.7944560844389300103, 0.000000000000000000, 0.6073216033519338586 ) ) ;
#8338 = CARTESIAN_POINT ( 'NONE',  ( 13.30359063182643808, 144.2231605954833924, 276.4307627107033341 ) ) ;
#8339 = AXIS2_PLACEMENT_3D ( 'NONE', #1075, #4833, #6237 ) ;
#8340 = CARTESIAN_POINT ( 'NONE',  ( 12.90979805384899848, 187.4290109168892968, 322.9333241855586607 ) ) ;
#8341 = EDGE_CURVE ( 'NONE', #21383, #3254, #5502, .T. ) ;
#8342 = EDGE_CURVE ( 'NONE', #10602, #2469, #1842, .T. ) ;
#8343 = DIRECTION ( 'NONE',  ( -0.1296504907605104673, -0.005475273188900901117, -0.9915446392518421082 ) ) ;
#8344 = DIRECTION ( 'NONE',  ( -1.458023040593674845E-16, 0.000000000000000000, -1.000000000000000000 ) ) ;
#8345 = CARTESIAN_POINT ( 'NONE',  ( -12.58378492319879705, 109.7167104967248434, 130.3428598364639299 ) ) ;
#8346 = ORIENTED_EDGE ( 'NONE', *, *, #3198, .F. ) ;
#8347 = DIRECTION ( 'NONE',  ( 1.387778780781444256E-14, 0.000000000000000000, 1.000000000000000000 ) ) ;
#8348 = DIRECTION ( 'NONE',  ( -0.1136178953597578312, 0.9935164314186356593, -0.004009283626633664867 ) ) ;
#8349 = DIRECTION ( 'NONE',  ( -6.938893903907215756E-15, 0.000000000000000000, 1.000000000000000000 ) ) ;
#8350 = CARTESIAN_POINT ( 'NONE',  ( 163.9999999999998863, 18.00000000000000355, 8.000000000002229328 ) ) ;
#8351 = COLOUR_RGB ( '', 0.31764706, 0.68627451, 0.89019608) ;
#8352 = CARTESIAN_POINT ( 'NONE',  ( -27.75997226120959382, 324.1497707426385659, 317.2680019637485316 ) ) ;
#8353 = EDGE_CURVE ( 'NONE', #13470, #17822, #4385, .T. ) ;
#8354 = EDGE_CURVE ( 'NONE', #22481, #8451, #15395, .T. ) ;
#8355 = CARTESIAN_POINT ( 'NONE',  ( -6.192786246109101889, 70.35631045439366460, -98.23155991399221421 ) ) ;
#8356 = CARTESIAN_POINT ( 'NONE',  ( -50.59678745519813958, 169.7436444119130101, -45.84920262148475700 ) ) ;
#8357 = FACE_BOUND ( 'NONE', #22078, .T. ) ;
#8358 = EDGE_CURVE ( 'NONE', #18942, #17822, #21986, .T. ) ;
#8359 = PRODUCT_CONTEXT ( 'NONE', #16460, 'mechanical' ) ;
#8360 = CIRCLE ( 'NONE', #3966, 3.399999999999992806 ) ;
#8361 = VERTEX_POINT ( 'NONE', #20647 ) ;
#8362 = DIRECTION ( 'NONE',  ( 0.01292394549866727679, 0.005513023399720742325, 0.9999012842304692006 ) ) ;
#8363 = CARTESIAN_POINT ( 'NONE',  ( 45.23639694205829898, 173.1024896994836411, 17.99878014425653561 ) ) ;
#8364 = DIRECTION ( 'NONE',  ( -0.4397038457472313144, 0.000000000000000000, -0.8981428216242086648 ) ) ;
#8365 = CYLINDRICAL_SURFACE ( 'NONE', #18059, 22.50000000000000000 ) ;
#8366 = CARTESIAN_POINT ( 'NONE',  ( -38.79736811520099593, 127.3639955235004777, 248.0530059773089420 ) ) ;
#8367 = ADVANCED_FACE ( 'NONE', ( #18924 ), #3531, .T. ) ;
#8368 = DIRECTION ( 'NONE',  ( 0.9999164797902015955, 6.965998958219364448E-18, -0.01292414190464157182 ) ) ;
#8369 = LINE ( 'NONE', #1290, #9412 ) ;
#8370 = CIRCLE ( 'NONE', #2519, 102.6746853779045381 ) ;
#8371 =( REPRESENTATION_RELATIONSHIP ('NONE','NONE', #11808, #14914 ) REPRESENTATION_RELATIONSHIP_WITH_TRANSFORMATION ( #21655 )SHAPE_REPRESENTATION_RELATIONSHIP( ) );
#8372 = ORIENTED_EDGE ( 'NONE', *, *, #2650, .T. ) ;
#8373 = ADVANCED_FACE ( 'NONE', ( #1480 ), #4907, .T. ) ;
#8374 = CARTESIAN_POINT ( 'NONE',  ( -88.18706637290659955, 88.71869973106718987, 50.32066939225188662 ) ) ;
#8375 = ORIENTED_EDGE ( 'NONE', *, *, #20997, .T. ) ;
#8376 = DIRECTION ( 'NONE',  ( -0.000000000000000000, -1.000000000000000000, 0.000000000000000000 ) ) ;
#8377 = DIRECTION ( 'NONE',  ( -7.125109674160325297E-05, 0.9999848031710253382, -0.005512562950849327591 ) ) ;
#8378 = LINE ( 'NONE', #11852, #15715 ) ;
#8379 = CARTESIAN_POINT ( 'NONE',  ( 90.40889375659912730, 78.43035437438885538, -33.17122784026042837 ) ) ;
#8380 = ORIENTED_EDGE ( 'NONE', *, *, #6709, .F. ) ;
#8381 = CARTESIAN_POINT ( 'NONE',  ( -37.99682623202767928, 170.0000000000000284, 0.4911173923763579863 ) ) ;
#8382 = VECTOR ( 'NONE', #7644, 1000.000000000000000 ) ;
#8383 = EDGE_LOOP ( 'NONE', ( #9522, #15270, #4114, #12068 ) ) ;
#8384 = DIRECTION ( 'NONE',  ( -1.000000000000000000, 0.000000000000000000, 0.000000000000000000 ) ) ;
#8385 = FACE_OUTER_BOUND ( 'NONE', #5343, .T. ) ;
#8386 = VECTOR ( 'NONE', #3116, 1000.000000000000114 ) ;
#8387 = ORIENTED_EDGE ( 'NONE', *, *, #1718, .T. ) ;
#8388 = SURFACE_STYLE_USAGE ( .BOTH. , #14977 ) ;
#8389 = CARTESIAN_POINT ( 'NONE',  ( -89.95410508456485843, 88.80250242289463358, 52.38924411555903760 ) ) ;
#8390 = EDGE_CURVE ( 'NONE', #13470, #5262, #22457, .T. ) ;
#8391 = ORIENTED_EDGE ( 'NONE', *, *, #11904, .F. ) ;
#8392 = DIRECTION ( 'NONE',  ( -0.8588562297929583922, -0.3902276408394327323, 0.3317956673477156504 ) ) ;
#8393 = CARTESIAN_POINT ( 'NONE',  ( -47.41227093301287709, 106.1692389898096280, 200.5308336077392823 ) ) ;
#8394 = CYLINDRICAL_SURFACE ( 'NONE', #4698, 8.000000000000003553 ) ;
#8395 = AXIS2_PLACEMENT_3D ( 'NONE', #21428, #17899, #16066 ) ;
#8396 = CARTESIAN_POINT ( 'NONE',  ( -88.16340328200274712, 88.26057420812728083, 52.92017833001973770 ) ) ;
#8397 = CARTESIAN_POINT ( 'NONE',  ( -88.55404276674165942, 79.97526064827543735, 31.48874835467963607 ) ) ;
#8398 = DIRECTION ( 'NONE',  ( 0.9232306267972774094, 0.000000000000000000, -0.3842462878721227826 ) ) ;
#8399 = VERTEX_POINT ( 'NONE', #20756 ) ;
#8400 = EDGE_CURVE ( 'NONE', #7605, #12053, #5012, .T. ) ;
#8401 = ORIENTED_EDGE ( 'NONE', *, *, #22325, .F. ) ;
#8402 = AXIS2_PLACEMENT_3D ( 'NONE', #15294, #20416, #8023 ) ;
#8403 = ORIENTED_EDGE ( 'NONE', *, *, #1489, .T. ) ;
#8404 = FACE_OUTER_BOUND ( 'NONE', #18039, .T. ) ;
#8405 = DIRECTION ( 'NONE',  ( -0.01292414190464044946, -4.254338997373069277E-37, -0.9999164797902017066 ) ) ;
#8406 = CARTESIAN_POINT ( 'NONE',  ( 88.42085790543281121, 80.22997387171264450, -32.23265953185130428 ) ) ;
#8407 = LINE ( 'NONE', #15563, #10695 ) ;
#8408 = DIRECTION ( 'NONE',  ( 0.000000000000000000, 0.000000000000000000, 1.000000000000000000 ) ) ;
#8409 = ORIENTED_EDGE ( 'NONE', *, *, #3491, .F. ) ;
#8410 = FACE_OUTER_BOUND ( 'NONE', #14511, .T. ) ;
#8411 = CARTESIAN_POINT ( 'NONE',  ( -158.3970384574724051, 1.999999999999998224, 62.74304228515463677 ) ) ;
#8412 = ORIENTED_EDGE ( 'NONE', *, *, #2177, .F. ) ;
#8413 = CIRCLE ( 'NONE', #10249, 2.000000000000003997 ) ;
#8414 = ORIENTED_EDGE ( 'NONE', *, *, #29, .F. ) ;
#8415 = AXIS2_PLACEMENT_3D ( 'NONE', #13819, #14051, #11982 ) ;
#8416 = CARTESIAN_POINT ( 'NONE',  ( -21.30129866354425516, 189.4444907833431273, -100.5497760856508478 ) ) ;
#8417 = EDGE_CURVE ( 'NONE', #4942, #3481, #8931, .T. ) ;
#8418 = ADVANCED_FACE ( 'NONE', ( #8923 ), #10652, .F. ) ;
#8419 = AXIS2_PLACEMENT_3D ( 'NONE', #17110, #1375, #8349 ) ;
#8421 = VERTEX_POINT ( 'NONE', #5356 ) ;
#8420 = VERTEX_POINT ( 'NONE', #2269 ) ;
#8422 = PLANE ( 'NONE',  #673 ) ;
#8423 = CARTESIAN_POINT ( 'NONE',  ( -89.90382325080345538, 72.53934035976358530, 61.83857552320039730 ) ) ;
#8424 = DIRECTION ( 'NONE',  ( 7.125109674403277385E-05, -0.9999848031710253382, 0.005512562950848281552 ) ) ;
#8425 = CARTESIAN_POINT ( 'NONE',  ( -91.74710091628168129, 71.28171241778764511, -60.68341510339269007 ) ) ;
#8426 = CARTESIAN_POINT ( 'NONE',  ( 13.01890817498768449, 190.3110758050131892, 320.8522954438618058 ) ) ;
#8427 = CARTESIAN_POINT ( 'NONE',  ( 42.95143350392208248, 94.48610424851695200, 82.84186520041141932 ) ) ;
#8428 = FACE_OUTER_BOUND ( 'NONE', #18522, .T. ) ;
#8429 = DIRECTION ( 'NONE',  ( 0.01292394549866738955, 0.005513023399720468239, 0.9999012842304693116 ) ) ;
#8430 = LINE ( 'NONE', #3259, #10819 ) ;
#8431 = CIRCLE ( 'NONE', #5856, 2.000000000000004885 ) ;
#8432 = CIRCLE ( 'NONE', #17626, 8.000000000000014211 ) ;
#8433 = CYLINDRICAL_SURFACE ( 'NONE', #12864, 7.499999999999991118 ) ;
#8434 = PRODUCT_DEFINITION_FORMATION_WITH_SPECIFIED_SOURCE ( 'ANY', '', #18346, .NOT_KNOWN. ) ;
#8435 = CARTESIAN_POINT ( 'NONE',  ( -39.99335306980157867, 94.48610424851698042, 83.91394493266459165 ) ) ;
#8436 = AXIS2_PLACEMENT_3D ( 'NONE', #5807, #12841, #7435 ) ;
#8437 = DIRECTION ( 'NONE',  ( -0.01292394549866750231, -0.005513023399722823126, -0.9999012842304692006 ) ) ;
#8438 = ORIENTED_EDGE ( 'NONE', *, *, #22223, .F. ) ;
#8439 = CARTESIAN_POINT ( 'NONE',  ( -9.804288294571927409, 187.7022783261437837, 321.1616740932373091 ) ) ;
#8440 = ORIENTED_EDGE ( 'NONE', *, *, #20658, .F. ) ;
#8441 = ADVANCED_FACE ( 'NONE', ( #19489 ), #14355, .T. ) ;
#8442 = AXIS2_PLACEMENT_3D ( 'NONE', #2554, #6105, #7719 ) ;
#8443 = DIRECTION ( 'NONE',  ( -0.000000000000000000, -1.000000000000000000, -0.000000000000000000 ) ) ;
#8444 = VECTOR ( 'NONE', #19646, 1000.000000000000227 ) ;
#8445 = ORIENTED_EDGE ( 'NONE', *, *, #5276, .T. ) ;
#8446 = CARTESIAN_POINT ( 'NONE',  ( -0.9086064320094255908, 327.1909312704538024, 309.9468142364838741 ) ) ;
#8447 = DIRECTION ( 'NONE',  ( 7.125109674403277385E-05, -0.9999848031710253382, 0.005512562950848281552 ) ) ;
#8448 = AXIS2_PLACEMENT_3D ( 'NONE', #1684, #19118, #6610 ) ;
#8449 = ORIENTED_EDGE ( 'NONE', *, *, #11190, .T. ) ;
#8450 = CARTESIAN_POINT ( 'NONE',  ( 14.04062050856939337, 186.9464262198503377, 322.8169914968837588 ) ) ;
#8451 = VERTEX_POINT ( 'NONE', #17687 ) ;
#8452 = CARTESIAN_POINT ( 'NONE',  ( 109.9190928854304588, 75.16976796352440715, 4.372055995853181720 ) ) ;
#8453 = ORIENTED_EDGE ( 'NONE', *, *, #1761, .T. ) ;
#8454 = PLANE ( 'NONE',  #19947 ) ;
#8455 = ORIENTED_EDGE ( 'NONE', *, *, #13506, .T. ) ;
#8456 = DIRECTION ( 'NONE',  ( -7.125109674081160920E-05, 0.9999848031710253382, -0.005512562950849312846 ) ) ;
#8457 = AXIS2_PLACEMENT_3D ( 'NONE', #10078, #2939, #22541 ) ;
#8458 = CARTESIAN_POINT ( 'NONE',  ( 3.982207582136937596, 166.6986315483347028, 308.0958888182936448 ) ) ;
#8459 = CARTESIAN_POINT ( 'NONE',  ( 43.19578322759555533, 127.3639955235004777, 246.9932263411283486 ) ) ;
#8460 = AXIS2_PLACEMENT_3D ( 'NONE', #22175, #13707, #17144 ) ;
#8461 = DIRECTION ( 'NONE',  ( 0.01292414190464131335, 0.000000000000000000, 0.9999164797902017066 ) ) ;
#8462 = CIRCLE ( 'NONE', #2970, 3.399999999999991918 ) ;
#8463 = DIRECTION ( 'NONE',  ( 7.125109674403277385E-05, -0.9999848031710253382, 0.005512562950848281552 ) ) ;
#8464 = EDGE_LOOP ( 'NONE', ( #620, #3032, #4088, #19026 ) ) ;
#8465 = CARTESIAN_POINT ( 'NONE',  ( 17.46478692018636636, 177.6255169206013989, 113.2244034703209365 ) ) ;
#8466 = ADVANCED_FACE ( 'NONE', ( #438 ), #13596, .F. ) ;
#8467 = DIRECTION ( 'NONE',  ( 0.01292394549866739996, 0.005513023399721131770, 0.9999012842304692006 ) ) ;
#8468 = CARTESIAN_POINT ( 'NONE',  ( -146.5000000000000000, 1.999999999999998224, 10.00000000000002487 ) ) ;
#8469 = ORIENTED_EDGE ( 'NONE', *, *, #9794, .F. ) ;
#8470 = VECTOR ( 'NONE', #20226, 1000.000000000000000 ) ;
#8471 = CARTESIAN_POINT ( 'NONE',  ( 158.3970384574715808, 1.999999999999998224, 62.74304228515676130 ) ) ;
#8472 = CARTESIAN_POINT ( 'NONE',  ( -14.56978029430814026, 147.5825162344054888, 276.9379655111616785 ) ) ;
#8473 = CARTESIAN_POINT ( 'NONE',  ( 13.28235005706528682, 159.1720975239875884, 299.5163413053770682 ) ) ;
#8474 = LINE ( 'NONE', #22472, #8526 ) ;
#8475 = AXIS2_PLACEMENT_3D ( 'NONE', #4245, #596, #9311 ) ;
#8476 = ORIENTED_EDGE ( 'NONE', *, *, #15855, .T. ) ;
#8477 = CARTESIAN_POINT ( 'NONE',  ( -16.77414143088337184, 138.3748544051812246, 249.7078392314084567 ) ) ;
#8478 = PLANE ( 'NONE',  #22581 ) ;
#8479 = EDGE_CURVE ( 'NONE', #1318, #20578, #3287, .T. ) ;
#8480 = ORIENTED_EDGE ( 'NONE', *, *, #19361, .T. ) ;
#8481 = CARTESIAN_POINT ( 'NONE',  ( -90.16222517276825954, 87.23703400121539175, 51.25429106922742051 ) ) ;
#8482 = ORIENTED_EDGE ( 'NONE', *, *, #8111, .T. ) ;
#8483 = SHAPE_REPRESENTATION_RELATIONSHIP ( 'NONE' , 'NONE' ,  #21177, #6108 ) ;
#8484 = DIRECTION ( 'NONE',  ( 0.9999164797902015955, 0.000000000000000000, -0.01292414190464118845 ) ) ;
#8485 = CARTESIAN_POINT ( 'NONE',  ( 106.0939156777172485, 70.76422767839095229, 29.05317630099624893 ) ) ;
#8486 = LINE ( 'NONE', #6665, #1182 ) ;
#8487 = EDGE_CURVE ( 'NONE', #12028, #10294, #4406, .T. ) ;
#8488 = EDGE_LOOP ( 'NONE', ( #20602, #6147, #18172, #7626 ) ) ;
#8489 = CYLINDRICAL_SURFACE ( 'NONE', #13706, 3.399999999999991918 ) ;
#8490 = DIRECTION ( 'NONE',  ( -7.125109674403276030E-05, 0.9999848031710252272, -0.005512562950848280685 ) ) ;
#8491 = AXIS2_PLACEMENT_3D ( 'NONE', #13212, #8255, #20181 ) ;
#8492 = VERTEX_POINT ( 'NONE', #17808 ) ;
#8493 = VECTOR ( 'NONE', #8443, 1000.000000000000000 ) ;
#8494 = AXIS2_PLACEMENT_3D ( 'NONE', #9792, #8496, #16808 ) ;
#8495 = DIRECTION ( 'NONE',  ( -0.9999164797902017066, 0.000000000000000000, 0.01292414190463832269 ) ) ;
#8496 = DIRECTION ( 'NONE',  ( -0.9999164797902017066, -6.965998958219365988E-18, 0.01292414190464157356 ) ) ;
#8497 = ORIENTED_EDGE ( 'NONE', *, *, #16740, .F. ) ;
#8498 = EDGE_CURVE ( 'NONE', #17745, #4445, #10050, .T. ) ;
#8499 = CARTESIAN_POINT ( 'NONE',  ( -14.37471740060550118, 109.6998846769365628, 127.3137863664913425 ) ) ;
#8500 = CARTESIAN_POINT ( 'NONE',  ( -90.08563665347566030, 88.51714521506588085, 52.72240440167576025 ) ) ;
#8501 = EDGE_CURVE ( 'NONE', #4637, #9075, #16316, .T. ) ;
#8502 = AXIS2_PLACEMENT_3D ( 'NONE', #16239, #8851, #12546 ) ;
#8503 = EDGE_CURVE ( 'NONE', #13554, #7434, #15060, .T. ) ;
#8505 = VERTEX_POINT ( 'NONE', #14236 ) ;
#8504 = ORIENTED_EDGE ( 'NONE', *, *, #4403, .T. ) ;
#8506 = APPLICATION_CONTEXT ( 'automotive_design' ) ;
#8507 = EDGE_LOOP ( 'NONE', ( #18198, #5678, #12676, #4325, #20777, #11352, #8848, #1845 ) ) ;
#8508 = DIRECTION ( 'NONE',  ( 0.3101392564284310427, 0.9506461370142480494, -0.009250070373107139796 ) ) ;
#8509 = CARTESIAN_POINT ( 'NONE',  ( 158.3970384574715524, 20.00000000000000000, -62.74304228515679682 ) ) ;
#8510 = DIRECTION ( 'NONE',  ( 0.000000000000000000, 1.000000000000000000, 0.000000000000000000 ) ) ;
#8511 = SURFACE_SIDE_STYLE ('',( #13710 ) ) ;
#8512 = AXIS2_PLACEMENT_3D ( 'NONE', #9826, #6820, #4530 ) ;
#8513 = CARTESIAN_POINT ( 'NONE',  ( 84.91238002074454982, 75.00865516402794242, -2.421554962614585360 ) ) ;
#8514 = VECTOR ( 'NONE', #18949, 1000.000000000000227 ) ;
#8515 = CARTESIAN_POINT ( 'NONE',  ( 58.87600894486503478, 126.5883500096209815, 106.0876318414197499 ) ) ;
#8516 = ADVANCED_FACE ( 'NONE', ( #1932 ), #14122, .F. ) ;
#8517 = ORIENTED_EDGE ( 'NONE', *, *, #13583, .T. ) ;
#8518 = ORIENTED_EDGE ( 'NONE', *, *, #9794, .T. ) ;
#8519 = CARTESIAN_POINT ( 'NONE',  ( -6.151324038728556154, 188.8277583064068779, 276.4336127016060800 ) ) ;
#8520 = CARTESIAN_POINT ( 'NONE',  ( 49.99439896757524338, 189.9996960634205436, -0.7564583542491037926 ) ) ;
#8521 = CARTESIAN_POINT ( 'NONE',  ( -55.40268456415260800, 1.999999999999998224, 113.1659955246496025 ) ) ;
#8522 = CARTESIAN_POINT ( 'NONE',  ( -59.58073369746166748, 114.2548767969622077, 164.8171369447040320 ) ) ;
#8523 = CARTESIAN_POINT ( 'NONE',  ( -11.42851267050998132, 147.5070834042510342, 278.6502049059965884 ) ) ;
#8524 = ADVANCED_FACE ( 'NONE', ( #17912 ), #21537, .F. ) ;
#8525 = ORIENTED_EDGE ( 'NONE', *, *, #247, .T. ) ;
#8526 = VECTOR ( 'NONE', #22580, 999.9999999999998863 ) ;
#8527 = DIRECTION ( 'NONE',  ( 0.01292414190464217898, 1.902755938799531885E-22, 0.9999164797902015955 ) ) ;
#8528 = CARTESIAN_POINT ( 'NONE',  ( 90.75111155332047019, 98.75957274858882329, 62.16377225325069844 ) ) ;
#8529 = DIRECTION ( 'NONE',  ( 2.025474946048326158E-22, -1.000000000000000000, 1.876735158486679638E-22 ) ) ;
#8530 = EDGE_LOOP ( 'NONE', ( #11472, #11034, #3246, #4628 ) ) ;
#8531 = CIRCLE ( 'NONE', #15532, 14.36898871458905269 ) ;
#8532 = ORIENTED_EDGE ( 'NONE', *, *, #9921, .T. ) ;
#8533 = EDGE_CURVE ( 'NONE', #4095, #5262, #17247, .T. ) ;
#8534 = CIRCLE ( 'NONE', #15163, 5.099999999999992539 ) ;
#8535 = LINE ( 'NONE', #3034, #15236 ) ;
#8536 = EDGE_CURVE ( 'NONE', #6699, #8927, #9159, .T. ) ;
#8537 = VERTEX_POINT ( 'NONE', #5466 ) ;
#8538 = DIRECTION ( 'NONE',  ( -0.000000000000000000, -1.000000000000000000, -0.000000000000000000 ) ) ;
#8539 = CARTESIAN_POINT ( 'NONE',  ( -9.128127327470902941, 109.6831586031284758, 124.2118453865659546 ) ) ;
#8540 = DIRECTION ( 'NONE',  ( -0.000000000000000000, -1.000000000000000000, 0.000000000000000000 ) ) ;
#8541 = CARTESIAN_POINT ( 'NONE',  ( 162.0000000000000000, 2.000000000000000000, 2.222801351277976832E-12 ) ) ;
#8542 = VERTEX_POINT ( 'NONE', #9146 ) ;
#8543 = SURFACE_SIDE_STYLE ('',( #19743 ) ) ;
#8544 = DIRECTION ( 'NONE',  ( 0.9999164797902017066, 6.965998958219365988E-18, -0.01292414190464157356 ) ) ;
#8545 = CARTESIAN_POINT ( 'NONE',  ( 3.577593693774890227, 190.2936927735998154, 294.5394986654007994 ) ) ;
#8546 = CARTESIAN_POINT ( 'NONE',  ( 11.84242116924777299, 187.7489332779533981, 304.8764670816960347 ) ) ;
#8547 = CIRCLE ( 'NONE', #14071, 4.199999999999997513 ) ;
#8548 = CARTESIAN_POINT ( 'NONE',  ( -91.23603883849614249, 79.86121811340019860, -30.82342686631250217 ) ) ;
#8549 = CIRCLE ( 'NONE', #6358, 2.499999999999988010 ) ;
#8550 = CARTESIAN_POINT ( 'NONE',  ( -58.84871535152515065, 114.6403824866543175, 163.0520739249805899 ) ) ;
#8551 = ADVANCED_FACE ( 'NONE', ( #16198, #12503 ), #14581, .T. ) ;
#8552 = CARTESIAN_POINT ( 'NONE',  ( -90.17340641399441381, 87.01242838177741135, 51.39043932755232902 ) ) ;
#8553 = CARTESIAN_POINT ( 'NONE',  ( -8.612176237581371296, 185.3530072361552641, 305.1640391583723044 ) ) ;
#8554 = VERTEX_POINT ( 'NONE', #5701 ) ;
#8555 = AXIS2_PLACEMENT_3D ( 'NONE', #15301, #3094, #5365 ) ;
#8556 = CIRCLE ( 'NONE', #14826, 2.499999999999988010 ) ;
#8557 = DIRECTION ( 'NONE',  ( 2.025474946048326158E-22, -1.000000000000000000, 1.876735158486679638E-22 ) ) ;
#8558 = EDGE_LOOP ( 'NONE', ( #7932, #21056 ) ) ;
#8559 = ADVANCED_FACE ( 'NONE', ( #19817 ), #12116, .F. ) ;
#8560 = AXIS2_PLACEMENT_3D ( 'NONE', #9071, #10704, #1749 ) ;
#8561 = VECTOR ( 'NONE', #11642, 1000.000000000000000 ) ;
#8562 = CARTESIAN_POINT ( 'NONE',  ( 0.000000000000000000, 45.00000000000000000, 0.000000000000000000 ) ) ;
#8563 = PRODUCT_DEFINITION_CONTEXT ( 'detailed design', #12488, 'design' ) ;
#8564 = CARTESIAN_POINT ( 'NONE',  ( 12.08460136693709153, 159.1320474315246543, 323.5344127036669875 ) ) ;
#8565 = CARTESIAN_POINT ( 'NONE',  ( -104.8202145123291018, 69.99999999999998579, 33.35749735200943178 ) ) ;
#8566 = CARTESIAN_POINT ( 'NONE',  ( -56.11381622223437660, 118.5884715842524315, 107.6180086640604543 ) ) ;
#8567 = VERTEX_POINT ( 'NONE', #16758 ) ;
#8568 = DIRECTION ( 'NONE',  ( -7.125109674161447446E-05, 0.9999848031710253382, -0.005512562950850309444 ) ) ;
#8569 = AXIS2_PLACEMENT_3D ( 'NONE', #19427, #17391, #5522 ) ;
#8570 = CARTESIAN_POINT ( 'NONE',  ( -51.99565694909051672, 170.0000000000000284, 0.6720553790413400508 ) ) ;
#8571 = CARTESIAN_POINT ( 'NONE',  ( 108.0150042066416347, 77.63434920764957781, 21.27676351751525274 ) ) ;
#8572 = EDGE_CURVE ( 'NONE', #16738, #14056, #8070, .T. ) ;
#8573 = DIRECTION ( 'NONE',  ( -0.01292414190464131335, 0.000000000000000000, -0.9999164797902017066 ) ) ;
#8574 = ADVANCED_FACE ( 'NONE', ( #6167 ), #22350, .F. ) ;
#8575 = LINE ( 'NONE', #4902, #17795 ) ;
#8576 = CIRCLE ( 'NONE', #12641, 4.400000000000003908 ) ;
#8577 = ORIENTED_EDGE ( 'NONE', *, *, #11320, .T. ) ;
#8578 = CARTESIAN_POINT ( 'NONE',  ( -54.94942802003276938, 118.9356788078023328, 170.5867196356439877 ) ) ;
#8579 = AXIS2_PLACEMENT_3D ( 'NONE', #21825, #2792, #14981 ) ;
#8580 = ORIENTED_EDGE ( 'NONE', *, *, #986, .F. ) ;
#8581 = CARTESIAN_POINT ( 'NONE',  ( -92.14659905926313854, 77.13858430795839638, 31.20924108170686040 ) ) ;
#8582 = CARTESIAN_POINT ( 'NONE',  ( 163.1715728752537018, 20.00000000000000000, 8.828427124748406740 ) ) ;
#8583 = CARTESIAN_POINT ( 'NONE',  ( 16.79209292077435123, 185.4001249148296893, 322.0628622613651260 ) ) ;
#8584 = LINE ( 'NONE', #3426, #1651 ) ;
#8585 = ORIENTED_EDGE ( 'NONE', *, *, #16391, .F. ) ;
#8586 = DIRECTION ( 'NONE',  ( 0.01292394549866738782, 0.005513023399720700692, 0.9999012842304693116 ) ) ;
#8587 = CARTESIAN_POINT ( 'NONE',  ( -41.56623493000981284, 72.00000000000000000, -82.46967996629571473 ) ) ;
#8588 = CARTESIAN_POINT ( 'NONE',  ( 58.09936094630035797, 143.2573102595451928, 45.99984121742717491 ) ) ;
#8589 = CARTESIAN_POINT ( 'NONE',  ( -46.77099456471874817, 129.3749911766419700, 250.1451765551053654 ) ) ;
#8590 = CARTESIAN_POINT ( 'NONE',  ( 21.59573423564103933, 55.00725983767638638, -133.0670891953131161 ) ) ;
#8591 = EDGE_LOOP ( 'NONE', ( #12621, #14269, #16261, #19878 ) ) ;
#8592 = AXIS2_PLACEMENT_3D ( 'NONE', #6383, #9359, #18118 ) ;
#8593 = DIRECTION ( 'NONE',  ( 0.9999164797902017066, 6.965998958219365988E-18, -0.01292414190464157356 ) ) ;
#8594 = CARTESIAN_POINT ( 'NONE',  ( -45.67488410632294915, 171.6105373975396162, -51.92370490599741117 ) ) ;
#8595 = DIRECTION ( 'NONE',  ( -0.9999164797902017066, -5.258382537605284335E-16, 0.01292414190464131508 ) ) ;
#8596 = CARTESIAN_POINT ( 'NONE',  ( -10.85595612533484911, 109.6999345499266525, 127.2773526115149281 ) ) ;
#8597 = ORIENTED_EDGE ( 'NONE', *, *, #20137, .F. ) ;
#8598 = CARTESIAN_POINT ( 'NONE',  ( -5.055008945778654450, 172.7557180373005679, 323.6808309321652928 ) ) ;
#8599 = DIRECTION ( 'NONE',  ( -0.01292394549866632963, -0.005513023399716958026, -0.9999012842304692006 ) ) ;
#8600 = ORIENTED_EDGE ( 'NONE', *, *, #19467, .T. ) ;
#8601 = CARTESIAN_POINT ( 'NONE',  ( 47.42520555854284225, 108.9831925648675934, -44.78095427109676052 ) ) ;
#8602 = VERTEX_POINT ( 'NONE', #9956 ) ;
#8603 = DIRECTION ( 'NONE',  ( 0.9999164797902017066, 2.001050586450178695E-22, -0.01292414190464131508 ) ) ;
#8604 = DIRECTION ( 'NONE',  ( 0.01292394549866733230, 0.005513023399720419666, 0.9999012842304692006 ) ) ;
#8605 = DIRECTION ( 'NONE',  ( -2.025474946048326158E-22, 1.000000000000000000, -1.876735158486679638E-22 ) ) ;
#8606 = ORIENTED_EDGE ( 'NONE', *, *, #11291, .T. ) ;
#8607 = CARTESIAN_POINT ( 'NONE',  ( 0.000000000000000000, 0.000000000000000000, 0.000000000000000000 ) ) ;
#8608 = CARTESIAN_POINT ( 'NONE',  ( -5.563703806604336499, 326.7005119474492290, 320.3383740725300299 ) ) ;
#8609 = EDGE_LOOP ( 'NONE', ( #6616, #18782, #8600, #15706 ) ) ;
#8610 = CARTESIAN_POINT ( 'NONE',  ( -1.589012106048833584, 327.1475487665277342, 318.4782710686421865 ) ) ;
#8611 = ORIENTED_EDGE ( 'NONE', *, *, #13936, .F. ) ;
#8612 = DIRECTION ( 'NONE',  ( -0.9999164797902017066, -2.001050586450178931E-22, 0.01292414190464131508 ) ) ;
#8613 = ADVANCED_FACE ( 'NONE', ( #7891 ), #4310, .T. ) ;
#8614 = CARTESIAN_POINT ( 'NONE',  ( -89.89702621265139726, 88.86943147588976899, 52.27963238237415311 ) ) ;
#8615 = CARTESIAN_POINT ( 'NONE',  ( 3.872354045398264777, 166.6517708494370709, 299.5967279023346350 ) ) ;
#8616 = CIRCLE ( 'NONE', #16729, 124.0000000000000000 ) ;
#8617 = ORIENTED_EDGE ( 'NONE', *, *, #12186, .F. ) ;
#8618 = EDGE_LOOP ( 'NONE', ( #9970, #18174, #1866, #22480 ) ) ;
#8619 = FACE_OUTER_BOUND ( 'NONE', #21912, .T. ) ;
#8620 = CARTESIAN_POINT ( 'NONE',  ( 91.21019055468687498, 72.00000000000000000, 28.82359390673205723 ) ) ;
#8621 = CARTESIAN_POINT ( 'NONE',  ( 41.59208321381912299, 91.17157287525387233, 84.46951292587608862 ) ) ;
#8622 = CARTESIAN_POINT ( 'NONE',  ( 84.38591728079271093, 75.03398072390710638, -3.646888635650151311 ) ) ;
#8623 = LINE ( 'NONE', #7143, #17400 ) ;
#8624 = VERTEX_POINT ( 'NONE', #4428 ) ;
#8625 = ORIENTED_EDGE ( 'NONE', *, *, #11910, .T. ) ;
#8626 = FACE_BOUND ( 'NONE', #8250, .T. ) ;
#8627 = CARTESIAN_POINT ( 'NONE',  ( -56.85751309718151703, 126.2713511641368171, 50.07958431720155090 ) ) ;
#8628 = CARTESIAN_POINT ( 'NONE',  ( 42.84128820176451313, 101.1708071963161615, 64.81746289747974288 ) ) ;
#8629 = CARTESIAN_POINT ( 'NONE',  ( 85.63433794141033673, 105.0000000000000000, 69.04172771111926465 ) ) ;
#8630 = ADVANCED_FACE ( 'NONE', ( #18339 ), #11681, .F. ) ;
#8631 = EDGE_CURVE ( 'NONE', #19271, #6314, #21277, .T. ) ;
#8632 = CARTESIAN_POINT ( 'NONE',  ( -105.7099399341925192, 78.83711888896343112, 30.42080736548454212 ) ) ;
#8633 = CARTESIAN_POINT ( 'NONE',  ( 0.000000000000000000, 0.000000000000000000, 0.000000000000000000 ) ) ;
#8634 = CARTESIAN_POINT ( 'NONE',  ( -13.92525281995234820, 325.7770340667113942, 328.4523304068723064 ) ) ;
#8635 = CIRCLE ( 'NONE', #4961, 3.999999999999999556 ) ;
#8636 = PRODUCT_DEFINITION_SHAPE ( 'NONE', 'NONE',  #22675 ) ;
#8637 = FACE_OUTER_BOUND ( 'NONE', #14758, .T. ) ;
#8638 = ORIENTED_EDGE ( 'NONE', *, *, #14489, .F. ) ;
#8639 = ORIENTED_EDGE ( 'NONE', *, *, #12685, .T. ) ;
#8640 = ORIENTED_EDGE ( 'NONE', *, *, #14627, .T. ) ;
#8641 = EDGE_CURVE ( 'NONE', #369, #16780, #12970, .T. ) ;
#8642 = DIRECTION ( 'NONE',  ( -0.000000000000000000, -1.000000000000000000, -0.000000000000000000 ) ) ;
#8644 = EDGE_LOOP ( 'NONE', ( #21791, #13796 ) ) ;
#8643 = ORIENTED_EDGE ( 'NONE', *, *, #3168, .T. ) ;
#8645 = EDGE_CURVE ( 'NONE', #10802, #12309, #13247, .T. ) ;
#8646 = PLANE ( 'NONE',  #17262 ) ;
#8647 = CARTESIAN_POINT ( 'NONE',  ( 4.019267399398602336, 144.9537609278173704, 294.7139688332605374 ) ) ;
#8648 = CARTESIAN_POINT ( 'NONE',  ( -56.11438623100815448, 126.5883500096207683, 107.5739081604535414 ) ) ;
#8649 = LINE ( 'NONE', #10854, #7473 ) ;
#8650 = PRODUCT ( 'Lead Screw Drive Shaft', 'Lead Screw Drive Shaft', '', ( #1384 ) ) ;
#8651 = CARTESIAN_POINT ( 'NONE',  ( 86.01272713495869482, 75.01355197838040567, -2.728429179322157783 ) ) ;
#8652 = CARTESIAN_POINT ( 'NONE',  ( 11.68933415262360676, 187.8362014856246560, 307.7594460564280894 ) ) ;
#8653 = CARTESIAN_POINT ( 'NONE',  ( -50.95650037043956360, 189.5905040570864912, -73.67951233157160118 ) ) ;
#8654 = ADVANCED_FACE ( 'NONE', ( #7777 ), #663, .T. ) ;
#8655 = CARTESIAN_POINT ( 'NONE',  ( -10.75874152970787634, 105.7413430127404439, 134.7986624950468126 ) ) ;
#8656 = EDGE_CURVE ( 'NONE', #16120, #5948, #9743, .T. ) ;
#8657 = DIRECTION ( 'NONE',  ( -2.025474946048326158E-22, 1.000000000000000000, -1.876735158486679638E-22 ) ) ;
#8658 = CARTESIAN_POINT ( 'NONE',  ( -8.403644388133985288, 185.4916053321884704, 305.1405741905838340 ) ) ;
#8659 = ORIENTED_EDGE ( 'NONE', *, *, #11484, .F. ) ;
#8660 = DIRECTION ( 'NONE',  ( 0.9909299940865190504, -0.1338359446631136318, -0.01207007604876911971 ) ) ;
#8661 = ORIENTED_EDGE ( 'NONE', *, *, #19103, .F. ) ;
#8662 = LINE ( 'NONE', #15951, #17278 ) ;
#8663 = ADVANCED_FACE ( 'NONE', ( #21870 ), #21762, .F. ) ;
#8664 = SURFACE_STYLE_FILL_AREA ( #18002 ) ;
#8665 = VERTEX_POINT ( 'NONE', #6403 ) ;
#8666 = CARTESIAN_POINT ( 'NONE',  ( -9.134655005754131807, 69.99999999999998579, -85.72312909216951482 ) ) ;
#8667 = CARTESIAN_POINT ( 'NONE',  ( -9.829296516163982034, 187.6860858752735908, 321.1599732488574546 ) ) ;
#8668 = CARTESIAN_POINT ( 'NONE',  ( 17.85676077817555552, 146.8644376350167420, 276.7956092302854358 ) ) ;
#8669 = EDGE_LOOP ( 'NONE', ( #18798, #21717, #16911, #7787 ) ) ;
#8670 = CARTESIAN_POINT ( 'NONE',  ( 15.88786633120246172, 188.4315875916928746, 320.0875345304690427 ) ) ;
#8671 = ORIENTED_EDGE ( 'NONE', *, *, #14196, .T. ) ;
#8672 = FACE_OUTER_BOUND ( 'NONE', #17352, .T. ) ;
#8673 = EDGE_CURVE ( 'NONE', #18526, #14240, #16529, .T. ) ;
#8674 = CARTESIAN_POINT ( 'NONE',  ( 106.2770331005257702, 78.91761970611437960, -28.37590941890325880 ) ) ;
#8675 = SURFACE_STYLE_USAGE ( .BOTH. , #20751 ) ;
#8676 = CARTESIAN_POINT ( 'NONE',  ( 67.44333765613016851, 145.1911235850904234, 33.86722133266570722 ) ) ;
#8677 = VERTEX_POINT ( 'NONE', #2833 ) ;
#8678 = CARTESIAN_POINT ( 'NONE',  ( 70.91392079944854743, 69.99999999999998579, 84.09052168258639881 ) ) ;
#8679 = VERTEX_POINT ( 'NONE', #16651 ) ;
#8680 = CARTESIAN_POINT ( 'NONE',  ( 85.01653497985981289, 104.3814432989690602, -69.80106575130697877 ) ) ;
#8681 = LINE ( 'NONE', #12283, #8767 ) ;
#8682 = CARTESIAN_POINT ( 'NONE',  ( -90.00000000000000000, 29.00000000000000355, 8.394090934816448357E-16 ) ) ;
#8683 = CARTESIAN_POINT ( 'NONE',  ( 15.14609095036742481, 186.2064079090589814, 305.7394825653286148 ) ) ;
#8684 = DIRECTION ( 'NONE',  ( -0.6074180324222083760, -7.300068142772954271E-18, 0.7943823600057675627 ) ) ;
#8685 = CARTESIAN_POINT ( 'NONE',  ( 41.61793149762840471, 69.99999999999998579, 86.46934588545650513 ) ) ;
#8686 = CARTESIAN_POINT ( 'NONE',  ( 8.732651047105484565, 144.7526087692596946, 274.6521818617012514 ) ) ;
#8687 = AXIS2_PLACEMENT_3D ( 'NONE', #13028, #21483, #4141 ) ;
#8688 = DIRECTION ( 'NONE',  ( -5.440186201345785633E-18, -1.000000000000000000, -1.334940939666367878E-17 ) ) ;
#8689 = EDGE_CURVE ( 'NONE', #6325, #3099, #10292, .T. ) ;
#8690 = ITEM_DEFINED_TRANSFORMATION ( 'NONE', 'NONE', #4400,  #6292 ) ;
#8691 = EDGE_CURVE ( 'NONE', #5449, #11742, #781, .T. ) ;
#8692 = CARTESIAN_POINT ( 'NONE',  ( 29.05310264022292444, 95.51270090492251086, 81.29561921768980426 ) ) ;
#8693 = CARTESIAN_POINT ( 'NONE',  ( 64.31884524158141403, 144.7109461922390778, -53.19708549627201677 ) ) ;
#8694 = CARTESIAN_POINT ( 'NONE',  ( -1.163172771417702478, 87.00000000000001421, -89.99248318111824574 ) ) ;
#8695 = DIRECTION ( 'NONE',  ( 0.01292394549866738608, 0.005513023399720699824, 0.9999012842304692006 ) ) ;
#8696 = DIRECTION ( 'NONE',  ( -0.01292394549866741384, -0.005513023399720269613, -0.9999012842304692006 ) ) ;
#8697 = ORIENTED_EDGE ( 'NONE', *, *, #19180, .T. ) ;
#8698 = LINE ( 'NONE', #21120, #13089 ) ;
#8699 = CARTESIAN_POINT ( 'NONE',  ( 59.65023440614042727, 143.9188730675116688, 165.9879953250834603 ) ) ;
#8700 = ORIENTED_EDGE ( 'NONE', *, *, #13529, .T. ) ;
#8701 = CARTESIAN_POINT ( 'NONE',  ( 47.50863050553487454, 109.5713193606044200, -44.78527523389898590 ) ) ;
#8702 = ORIENTED_EDGE ( 'NONE', *, *, #17652, .F. ) ;
#8703 = CARTESIAN_POINT ( 'NONE',  ( -52.59261083883858134, 113.4706157781613598, -45.51314101063805140 ) ) ;
#8704 = CARTESIAN_POINT ( 'NONE',  ( -12.58378492319879527, 109.7167104967248434, 130.3428598364639299 ) ) ;
#8705 = CARTESIAN_POINT ( 'NONE',  ( -12.64688860274155324, 109.6831087301383860, 124.2482791415423691 ) ) ;
#8706 = AXIS2_PLACEMENT_3D ( 'NONE', #15081, #12072, #8280 ) ;
#8707 = ORIENTED_EDGE ( 'NONE', *, *, #585, .T. ) ;
#8708 = CARTESIAN_POINT ( 'NONE',  ( 0.000000000000000000, 23.00000000000000000, 0.000000000000000000 ) ) ;
#8709 = DIRECTION ( 'NONE',  ( -0.000000000000000000, -1.000000000000000000, -0.000000000000000000 ) ) ;
#8710 = EDGE_LOOP ( 'NONE', ( #14140, #2318, #13734 ) ) ;
#8711 = CARTESIAN_POINT ( 'NONE',  ( -2.528315839145332866, 327.0432605512580722, 319.2538853862658925 ) ) ;
#8712 = VERTEX_POINT ( 'NONE', #4650 ) ;
#8713 = AXIS2_PLACEMENT_3D ( 'NONE', #6560, #16806, #8050 ) ;
#8714 = CYLINDRICAL_SURFACE ( 'NONE', #3238, 5.099999999999992539 ) ;
#8715 = EDGE_CURVE ( 'NONE', #17033, #2396, #7360, .T. ) ;
#8716 = CARTESIAN_POINT ( 'NONE',  ( -88.16708379909647419, 88.58102416753696673, 52.59057003169024824 ) ) ;
#8717 = DIRECTION ( 'NONE',  ( 0.9934404589540162256, 0.1135548637187057258, -0.01346653032742958084 ) ) ;
#8719 = ORIENTED_EDGE ( 'NONE', *, *, #14419, .F. ) ;
#8718 = ORIENTED_EDGE ( 'NONE', *, *, #1841, .T. ) ;
#8720 = ORIENTED_EDGE ( 'NONE', *, *, #13315, .T. ) ;
#8721 = FACE_OUTER_BOUND ( 'NONE', #20341, .T. ) ;
#8722 = FACE_OUTER_BOUND ( 'NONE', #8856, .T. ) ;
#8723 = ORIENTED_EDGE ( 'NONE', *, *, #15764, .T. ) ;
#8724 = FACE_OUTER_BOUND ( 'NONE', #11861, .T. ) ;
#8725 = CARTESIAN_POINT ( 'NONE',  ( 84.54811758989713155, 75.02636992936612614, -3.352151862290983608 ) ) ;
#8726 = DIRECTION ( 'NONE',  ( -7.125109674403837105E-05, 0.9999848031710252272, -0.005512562950847867821 ) ) ;
#8727 = CYLINDRICAL_SURFACE ( 'NONE', #4155, 2.000000000000000000 ) ;
#8728 = ORIENTED_EDGE ( 'NONE', *, *, #6869, .F. ) ;
#8729 = EDGE_LOOP ( 'NONE', ( #19939, #18243, #18960, #14611 ) ) ;
#8730 = CARTESIAN_POINT ( 'NONE',  ( 0.000000000000000000, 0.000000000000000000, -96.00000000000000000 ) ) ;
#8731 = CARTESIAN_POINT ( 'NONE',  ( -75.62605524907648658, 75.03814149158517921, 3.672988387105930119 ) ) ;
#8732 = CARTESIAN_POINT ( 'NONE',  ( -26.51496018000491617, 324.2983970019843696, 318.8161534577199632 ) ) ;
#8733 = CARTESIAN_POINT ( 'NONE',  ( -105.4775731789987674, 77.90269639574782445, 31.21677525025618039 ) ) ;
#8734 = CARTESIAN_POINT ( 'NONE',  ( -35.95309506732429128, 93.50464841319750064, -82.03286182426641915 ) ) ;
#8735 = CARTESIAN_POINT ( 'NONE',  ( 70.91392079944854743, 72.00000000000000000, 84.09052168258639881 ) ) ;
#8736 = AXIS2_PLACEMENT_3D ( 'NONE', #6565, #18735, #11632 ) ;
#8737 = CARTESIAN_POINT ( 'NONE',  ( 0.000000000000000000, 20.00000000000000000, 0.000000000000000000 ) ) ;
#8738 = CARTESIAN_POINT ( 'NONE',  ( -39.11273342774205730, 91.99797716581187501, -83.46418088055293083 ) ) ;
#8739 = VERTEX_POINT ( 'NONE', #2730 ) ;
#8740 = DIRECTION ( 'NONE',  ( 0.01292394549866733230, 0.005513023399720419666, 0.9999012842304692006 ) ) ;
#8741 = VERTEX_POINT ( 'NONE', #14694 ) ;
#8742 = EDGE_LOOP ( 'NONE', ( #903, #15900, #3968, #9123 ) ) ;
#8743 = UNCERTAINTY_MEASURE_WITH_UNIT (LENGTH_MEASURE( 1.000000000000000082E-05 ), #3324, 'distance_accuracy_value', 'NONE');
#8744 = CARTESIAN_POINT ( 'NONE',  ( 19.75068821775290218, 183.8270873257126539, 315.7595470900485566 ) ) ;
#8745 = VECTOR ( 'NONE', #8568, 999.9999999999998863 ) ;
#8746 = ADVANCED_FACE ( 'NONE', ( #12129 ), #3685, .T. ) ;
#8747 = EDGE_LOOP ( 'NONE', ( #6439, #19681, #4573, #9927 ) ) ;
#8748 = DIRECTION ( 'NONE',  ( 1.372099599554306628E-14, 0.000000000000000000, -1.000000000000000000 ) ) ;
#8749 = DIRECTION ( 'NONE',  ( 0.000000000000000000, -1.000000000000000000, 0.000000000000000000 ) ) ;
#8750 = EDGE_CURVE ( 'NONE', #11360, #7130, #4423, .T. ) ;
#8751 = CARTESIAN_POINT ( 'NONE',  ( -2.153876626942607952, 142.8329195585684488, 275.1002313843466709 ) ) ;
#8752 = CARTESIAN_POINT ( 'NONE',  ( 106.0833544754547972, 79.13355406794953240, -29.09322962842207971 ) ) ;
#8753 = CARTESIAN_POINT ( 'NONE',  ( -38.93929506000819174, 95.78282953318711179, 82.58910896792900758 ) ) ;
#8754 = ORIENTED_EDGE ( 'NONE', *, *, #20423, .F. ) ;
#8755 =( NAMED_UNIT ( * ) PLANE_ANGLE_UNIT ( ) SI_UNIT ( $, .RADIAN. ) );
#8756 = CARTESIAN_POINT ( 'NONE',  ( 84.06242043834124900, 75.11631364573369751, -5.795347279148256980 ) ) ;
#8757 = CARTESIAN_POINT ( 'NONE',  ( 15.72063276321387093, 185.9256727956241377, 308.2960514488045192 ) ) ;
#8758 = CARTESIAN_POINT ( 'NONE',  ( 91.32251664931575874, 80.22595383786462264, 29.89762933574812465 ) ) ;
#8759 = EDGE_CURVE ( 'NONE', #665, #1664, #13523, .T. ) ;
#8760 = CARTESIAN_POINT ( 'NONE',  ( 89.59766859896282654, 79.73843791202818920, 28.47398564242246977 ) ) ;
#8761 = ORIENTED_EDGE ( 'NONE', *, *, #20324, .T. ) ;
#8762 = VECTOR ( 'NONE', #11163, 1000.000000000000114 ) ;
#8763 = STYLED_ITEM ( 'NONE', ( #22281 ), #17335 ) ;
#8764 = ADVANCED_FACE ( 'NONE', ( #15485 ), #11918, .T. ) ;
#8765 = DIRECTION ( 'NONE',  ( 0.01292394549866740169, 0.005513023399720822990, 0.9999012842304693116 ) ) ;
#8766 = CARTESIAN_POINT ( 'NONE',  ( 1.721625266288852263, 105.0000000000000000, 109.9865264768483968 ) ) ;
#8767 = VECTOR ( 'NONE', #15730, 1000.000000000000114 ) ;
#8768 = ORIENTED_EDGE ( 'NONE', *, *, #3172, .T. ) ;
#8769 = CARTESIAN_POINT ( 'NONE',  ( -92.35175351209242933, 79.88298967447890675, -28.93780754488527052 ) ) ;
#8770 = ORIENTED_EDGE ( 'NONE', *, *, #2520, .F. ) ;
#8771 = ADVANCED_FACE ( 'NONE', ( #18796 ), #4987, .T. ) ;
#8772 = LINE ( 'NONE', #1912, #15093 ) ;
#8773 = EDGE_CURVE ( 'NONE', #22140, #6890, #11801, .T. ) ;
#8774 = EDGE_CURVE ( 'NONE', #11284, #10034, #3158, .T. ) ;
#8775 = LINE ( 'NONE', #12378, #303 ) ;
#8776 = EDGE_CURVE ( 'NONE', #4261, #12198, #19003, .T. ) ;
#8777 = TOROIDAL_SURFACE ( 'NONE', #16164, 8.000000000000014211, 2.000000000000000000 ) ;
#8778 = EDGE_CURVE ( 'NONE', #2070, #14285, #19058, .T. ) ;
#8779 = PLANE ( 'NONE',  #15194 ) ;
#8780 = VECTOR ( 'NONE', #866, 1000.000000000000114 ) ;
#8781 = CYLINDRICAL_SURFACE ( 'NONE', #9077, 2.000000000000004441 ) ;
#8782 = CARTESIAN_POINT ( 'NONE',  ( -37.41993370812568998, 108.0982075334647163, 199.8733557436837032 ) ) ;
#8783 = EDGE_LOOP ( 'NONE', ( #13163, #8697, #10453, #10142 ) ) ;
#8784 = DIRECTION ( 'NONE',  ( 0.4910069343201003411, -0.004767316193522950878, -0.8711426192914036859 ) ) ;
#8785 = VERTEX_POINT ( 'NONE', #10177 ) ;
#8786 = CARTESIAN_POINT ( 'NONE',  ( 20.99042507241804145, 140.4227465520236819, 76.49807275461785139 ) ) ;
#8787 = EDGE_CURVE ( 'NONE', #3170, #18739, #2606, .T. ) ;
#8788 = CARTESIAN_POINT ( 'NONE',  ( 52.77990858962370169, 106.8060942374655156, 70.25701329566173570 ) ) ;
#8789 = VERTEX_POINT ( 'NONE', #18899 ) ;
#8790 = CARTESIAN_POINT ( 'NONE',  ( -10.77448130880426724, 186.7844715323957416, 321.0194338377268650 ) ) ;
#8791 = VECTOR ( 'NONE', #16431, 1000.000000000000114 ) ;
#8792 = PLANE ( 'NONE',  #20261 ) ;
#8793 = LINE ( 'NONE', #18017, #16208 ) ;
#8794 = VERTEX_POINT ( 'NONE', #17090 ) ;
#8795 = CARTESIAN_POINT ( 'NONE',  ( 89.22767861003025303, 80.31838830481380853, 30.18953644180655971 ) ) ;
#8796 = ORIENTED_EDGE ( 'NONE', *, *, #8787, .F. ) ;
#8797 = EDGE_CURVE ( 'NONE', #3937, #2916, #15819, .T. ) ;
#8798 = CARTESIAN_POINT ( 'NONE',  ( 64.99457118636311748, 105.0000000000000000, -0.8400692238016954638 ) ) ;
#8799 = DIRECTION ( 'NONE',  ( 0.01292394549866738782, 0.005513023399721118760, 0.9999012842304692006 ) ) ;
#8800 = CARTESIAN_POINT ( 'NONE',  ( -15.55825634263874413, 177.7403479327107618, 314.6945671552619501 ) ) ;
#8801 = CONICAL_SURFACE ( 'NONE', #6617, 2.499999999999988010, 1.029744258676651425 ) ;
#8802 = EDGE_LOOP ( 'NONE', ( #12427, #652, #17135, #3206 ) ) ;
#8803 = VECTOR ( 'NONE', #16294, 1000.000000000000114 ) ;
#8804 = CARTESIAN_POINT ( 'NONE',  ( 17.16132609305713430, 185.1401191634033694, 321.7723388245965452 ) ) ;
#8805 = CIRCLE ( 'NONE', #11769, 4.999999999999990230 ) ;
#8806 = CARTESIAN_POINT ( 'NONE',  ( 36.94244151028511425, 91.99797716581187501, -84.44721085690419216 ) ) ;
#8807 = PRODUCT_DEFINITION_FORMATION_WITH_SPECIFIED_SOURCE ( 'ANY', '', #8081, .NOT_KNOWN. ) ;
#8808 = DIRECTION ( 'NONE',  ( -0.01292394549866632963, -0.005513023399716958026, -0.9999012842304692006 ) ) ;
#8809 = CARTESIAN_POINT ( 'NONE',  ( 394.9504264446939032, 92.58578643762699301, -89.52608615654116875 ) ) ;
#8810 = ADVANCED_FACE ( 'NONE', ( #6727, #13751 ), #20736, .T. ) ;
#8811 = AXIS2_PLACEMENT_3D ( 'NONE', #5671, #7064, #12709 ) ;
#8812 = CONTEXT_DEPENDENT_SHAPE_REPRESENTATION ( #16342, #1498 ) ;
#8813 = CARTESIAN_POINT ( 'NONE',  ( 19.84463980526027527, 7.270595330592044547, -12.14917202071510971 ) ) ;
#8814 = CARTESIAN_POINT ( 'NONE',  ( 49.99582398951007889, 170.0000000000000284, -0.6462070952321007367 ) ) ;
#8815 = DIRECTION ( 'NONE',  ( 0.9999164797902017066, 2.001050586450178931E-22, -0.01292414190464131508 ) ) ;
#8816 = CARTESIAN_POINT ( 'NONE',  ( 49.13077451860386446, 168.8134312302534283, 56.22586871687502708 ) ) ;
#8817 = CARTESIAN_POINT ( 'NONE',  ( -110.3452273899772962, 79.04398536104962147, -25.99873445483951073 ) ) ;
#8818 = CIRCLE ( 'NONE', #21649, 110.5324305509042233 ) ;
#8819 = EDGE_LOOP ( 'NONE', ( #12542, #17468, #17143, #8001 ) ) ;
#8820 = B_SPLINE_CURVE_WITH_KNOTS ( 'NONE', 3,
 ( #17367, #1626, #18051, #583, #5725, #2174, #18374, #11365 ),
 .UNSPECIFIED., .F., .F.,
 ( 4, 2, 2, 4 ),
 ( 0.005257893453559830781, 0.006567392922673205222, 0.007876892391786580530, 0.01049589133001331900 ),
 .UNSPECIFIED. ) ;
#8821 = CARTESIAN_POINT ( 'NONE',  ( 4.182528737366220106, 166.7840834110302808, 323.5943587238651276 ) ) ;
#8822 = DIRECTION ( 'NONE',  ( 0.1337561903331546953, 0.9909881666746205298, -0.007192708699472573526 ) ) ;
#8823 = AXIS2_PLACEMENT_3D ( 'NONE', #3730, #3506, #10522 ) ;
#8824 = ORIENTED_EDGE ( 'NONE', *, *, #10767, .T. ) ;
#8825 = CARTESIAN_POINT ( 'NONE',  ( 49.97753088104515484, 110.8699366255535637, -47.71756500317012240 ) ) ;
#8826 = VERTEX_POINT ( 'NONE', #22643 ) ;
#8827 =( NAMED_UNIT ( * ) PLANE_ANGLE_UNIT ( ) SI_UNIT ( $, .RADIAN. ) );
#8828 =( BOUNDED_SURFACE ( )  B_SPLINE_SURFACE ( 3, 2, ( 
 ( #22353, #6649, #18932 ),
 ( #13784, #6867, #14487 ),
 ( #17922, #12175, #21113 ),
 ( #5363, #14705, #14593 ) ),
 .UNSPECIFIED., .F., .F., .T. ) 
 B_SPLINE_SURFACE_WITH_KNOTS ( ( 4, 4 ),
 ( 3, 3 ),
 ( 5.799006443144740786, 5.860583945225279479 ),
 ( 0.000000000000000000, 1.000000000000000000 ),
 .UNSPECIFIED. ) 
 GEOMETRIC_REPRESENTATION_ITEM ( )  RATIONAL_B_SPLINE_SURFACE ( (
 ( 1.000000000000000000, 0.9016180287879261845, 1.000000000000000000),
 ( 1.000000000000000000, 0.9034913259101577943, 1.000000000000000000),
 ( 1.000000000000000000, 0.9052491015987668144, 1.000000000000000000),
 ( 1.000000000000000000, 0.9068900557993655465, 1.000000000000000000) ) ) 
 REPRESENTATION_ITEM ( '' )  SURFACE ( )  );
#8829 = CARTESIAN_POINT ( 'NONE',  ( -8.849534454763650970, 70.01899995639456620, -94.75705998267451946 ) ) ;
#8830 = FACE_OUTER_BOUND ( 'NONE', #6435, .T. ) ;
#8831 = FACE_OUTER_BOUND ( 'NONE', #15637, .T. ) ;
#8832 = CARTESIAN_POINT ( 'NONE',  ( 1.364374947835851710E-14, 55.00000000000000000, -9.836440897896405351E-15 ) ) ;
#8833 = ORIENTED_EDGE ( 'NONE', *, *, #32, .T. ) ;
#8834 = ORIENTED_EDGE ( 'NONE', *, *, #368, .T. ) ;
#8835 = EDGE_CURVE ( 'NONE', #20077, #16143, #6939, .T. ) ;
#8836 = CARTESIAN_POINT ( 'NONE',  ( -56.92213282467484703, 126.2437860471382294, 45.08007789604923232 ) ) ;
#8837 = AXIS2_PLACEMENT_3D ( 'NONE', #13397, #15000, #13161 ) ;
#8838 = CARTESIAN_POINT ( 'NONE',  ( -5.692304260892842471, 326.6858542223808968, 320.3505014899224648 ) ) ;
#8839 = DIRECTION ( 'NONE',  ( 0.9999164797902017066, 6.965998958219365988E-18, -0.01292414190464157356 ) ) ;
#8840 = ORIENTED_EDGE ( 'NONE', *, *, #13604, .F. ) ;
#8841 = CARTESIAN_POINT ( 'NONE',  ( 90.05385374424744782, 71.62832261676159362, -63.16885269282647641 ) ) ;
#8842 = VECTOR ( 'NONE', #8871, 999.9999999999998863 ) ;
#8843 = CARTESIAN_POINT ( 'NONE',  ( -90.06799945166942223, 87.57178311039056950, 51.04991898090875679 ) ) ;
#8844 = PRODUCT ( 'Holder', 'Holder', '', ( #2081 ) ) ;
#8845 = AXIS2_PLACEMENT_3D ( 'NONE', #1433, #17064, #11992 ) ;
#8846 = CONICAL_SURFACE ( 'NONE', #9591, 3.399999999999985700, 1.029744258676653201 ) ;
#8847 = VERTEX_POINT ( 'NONE', #8552 ) ;
#8848 = ORIENTED_EDGE ( 'NONE', *, *, #20873, .T. ) ;
#8849 = DIRECTION ( 'NONE',  ( 0.01292394549866739996, 0.005513023399721131770, 0.9999012842304692006 ) ) ;
#8850 = AXIS2_PLACEMENT_3D ( 'NONE', #623, #5659, #12695 ) ;
#8851 = DIRECTION ( 'NONE',  ( 0.8077751305149092342, -0.4220031449644174315, 0.4115977212786322004 ) ) ;
#8852 = PLANE ( 'NONE',  #2789 ) ;
#8853 = FACE_OUTER_BOUND ( 'NONE', #22505, .T. ) ;
#8854 = EDGE_LOOP ( 'NONE', ( #4733, #21539, #4951, #667 ) ) ;
#8855 = CARTESIAN_POINT ( 'NONE',  ( -14.82979117956944037, 177.4987173824078468, 90.64024647396865930 ) ) ;
#8856 = EDGE_LOOP ( 'NONE', ( #11986, #20886, #11431 ) ) ;
#8857 = LINE ( 'NONE', #12438, #6012 ) ;
#8858 = DIRECTION ( 'NONE',  ( -0.01292394549866741384, -0.005513023399720269613, -0.9999012842304692006 ) ) ;
#8859 = CARTESIAN_POINT ( 'NONE',  ( -13.82219771749447368, 164.6877133068229284, 314.3360916636659681 ) ) ;
#8860 = VECTOR ( 'NONE', #2414, 1000.000000000000114 ) ;
#8861 = ORIENTED_EDGE ( 'NONE', *, *, #4984, .F. ) ;
#8862 = CARTESIAN_POINT ( 'NONE',  ( 164.0000000000000000, 1.999999999999998224, -2.290411758281096087E-12 ) ) ;
#8863 = EDGE_CURVE ( 'NONE', #1291, #1333, #15593, .T. ) ;
#8864 = DIRECTION ( 'NONE',  ( -0.5698815422012539766, 0.5805244408402039369, 0.5815723527176038798 ) ) ;
#8865 = CARTESIAN_POINT ( 'NONE',  ( -90.00000000000000000, 0.000000000000000000, -10.99999999999999289 ) ) ;
#8866 = ADVANCED_FACE ( 'NONE', ( #21076 ), #10966, .F. ) ;
#8867 = AXIS2_PLACEMENT_3D ( 'NONE', #13229, #4470, #11500 ) ;
#8868 = LINE ( 'NONE', #19554, #13254 ) ;
#8869 = ORIENTED_EDGE ( 'NONE', *, *, #8645, .T. ) ;
#8870 = VECTOR ( 'NONE', #14513, 999.9999999999998863 ) ;
#8871 = DIRECTION ( 'NONE',  ( -7.125109674364536131E-05, 0.9999848031710253382, -0.005512562950849705760 ) ) ;
#8872 = ORIENTED_EDGE ( 'NONE', *, *, #4283, .F. ) ;
#8873 = VERTEX_POINT ( 'NONE', #185 ) ;
#8874 = ORIENTED_EDGE ( 'NONE', *, *, #10689, .T. ) ;
#8875 = DIRECTION ( 'NONE',  ( 0.9999164797902017066, 2.001050586450178931E-22, -0.01292414190464131508 ) ) ;
#8876 = AXIS2_PLACEMENT_3D ( 'NONE', #20036, #20268, #990 ) ;
#8877 = ORIENTED_EDGE ( 'NONE', *, *, #7756, .F. ) ;
#8878 = CIRCLE ( 'NONE', #7788, 6.500000000000000000 ) ;
#8879 = CARTESIAN_POINT ( 'NONE',  ( 0.000000000000000000, 37.00000000000000711, -96.00000000000000000 ) ) ;
#8880 = CARTESIAN_POINT ( 'NONE',  ( -16.00780723723847032, 316.4649337400251738, 414.4175034352881539 ) ) ;
#8881 = CARTESIAN_POINT ( 'NONE',  ( 51.05126519560737108, 95.51270090492249665, 81.01128809578769108 ) ) ;
#8882 = DIRECTION ( 'NONE',  ( 0.000000000000000000, 0.000000000000000000, -1.000000000000000000 ) ) ;
#8883 = DIRECTION ( 'NONE',  ( 0.009760756503427210282, -0.9999378516499566327, 0.005387065077606872227 ) ) ;
#8884 = CIRCLE ( 'NONE', #9246, 0.3999999999999986899 ) ;
#8885 = ORIENTED_EDGE ( 'NONE', *, *, #20711, .F. ) ;
#8886 = CARTESIAN_POINT ( 'NONE',  ( -64.28883878761487836, 83.29019440189557599, 55.44125366118053932 ) ) ;
#8887 = CARTESIAN_POINT ( 'NONE',  ( 81.53656681450840438, 75.19215068228483290, -7.093857522514749547 ) ) ;
#8888 = CARTESIAN_POINT ( 'NONE',  ( 12.35205150687213127, 187.5852105437413400, 307.7116188629170779 ) ) ;
#8889 = CARTESIAN_POINT ( 'NONE',  ( 91.61331032192579471, 77.62808270880876194, 29.62115891282539692 ) ) ;
#8890 = ORIENTED_EDGE ( 'NONE', *, *, #9966, .T. ) ;
#8891 = LINE ( 'NONE', #21405, #2595 ) ;
#8892 = AXIS2_PLACEMENT_3D ( 'NONE', #12637, #9035, #15981 ) ;
#8893 = EDGE_CURVE ( 'NONE', #17682, #21571, #8094, .T. ) ;
#8894 = VECTOR ( 'NONE', #7643, 1000.000000000000114 ) ;
#8895 = CARTESIAN_POINT ( 'NONE',  ( 49.39923347825703814, 108.3707227317548529, -46.80328957620831432 ) ) ;
#8896 = CYLINDRICAL_SURFACE ( 'NONE', #22022, 1.999999999999997780 ) ;
#8897 = ORIENTED_EDGE ( 'NONE', *, *, #15393, .T. ) ;
#8898 = CARTESIAN_POINT ( 'NONE',  ( -1.163172771417704698, 44.99899999999999523, -89.99248318111816047 ) ) ;
#8899 = ORIENTED_EDGE ( 'NONE', *, *, #10599, .T. ) ;
#8900 = CARTESIAN_POINT ( 'NONE',  ( -70.53865358177314704, 70.91952051830753589, -84.40563445996846781 ) ) ;
#8901 = EDGE_CURVE ( 'NONE', #12496, #5690, #9932, .T. ) ;
#8902 = DIRECTION ( 'NONE',  ( -0.01292394549866632963, -0.005513023399716958026, -0.9999012842304692006 ) ) ;
#8903 = VECTOR ( 'NONE', #7879, 1000.000000000000000 ) ;
#8904 = CIRCLE ( 'NONE', #14821, 1.989999999999999103 ) ;
#8905 = PLANE ( 'NONE',  #18820 ) ;
#8906 = CARTESIAN_POINT ( 'NONE',  ( 48.56920114533915722, 166.9610289984755127, 276.0150354541233924 ) ) ;
#8907 = ORIENTED_EDGE ( 'NONE', *, *, #22325, .T. ) ;
#8908 = CARTESIAN_POINT ( 'NONE',  ( 12.22168221341685879, 187.6955267389516564, 322.9731535519586032 ) ) ;
#8909 = ORIENTED_EDGE ( 'NONE', *, *, #20376, .F. ) ;
#8910 = CARTESIAN_POINT ( 'NONE',  ( -10.85624112972181621, 113.6998737626107641, 127.2553023597115498 ) ) ;
#8911 = LINE ( 'NONE', #19365, #19582 ) ;
#8912 = CARTESIAN_POINT ( 'NONE',  ( -6.855452219084264165, 165.4878736975560969, 88.60320152568080232 ) ) ;
#8913 = ORIENTED_EDGE ( 'NONE', *, *, #7379, .T. ) ;
#8914 = CARTESIAN_POINT ( 'NONE',  ( -8.736239094475285683, 185.1016632737992040, 323.2420184559757672 ) ) ;
#8915 = CARTESIAN_POINT ( 'NONE',  ( 13.80637996605699769, 137.5572120012638777, 100.9913744321402902 ) ) ;
#8916 = FACE_BOUND ( 'NONE', #16415, .T. ) ;
#8917 = VECTOR ( 'NONE', #5665, 1000.000000000000000 ) ;
#8918 = ORIENTED_EDGE ( 'NONE', *, *, #21673, .T. ) ;
#8919 = EDGE_CURVE ( 'NONE', #19509, #17777, #2120, .T. ) ;
#8920 = CARTESIAN_POINT ( 'NONE',  ( -1.523404093792848135, 158.5871283748866745, 324.7134023609685869 ) ) ;
#8921 = EDGE_CURVE ( 'NONE', #163, #17125, #7733, .T. ) ;
#8922 = EDGE_LOOP ( 'NONE', ( #16547, #17610, #17184 ) ) ;
#8923 = FACE_OUTER_BOUND ( 'NONE', #4219, .T. ) ;
#8924 = CARTESIAN_POINT ( 'NONE',  ( -10.85340889862633595, 73.95047783656255547, 127.4744267370078177 ) ) ;
#8925 = CARTESIAN_POINT ( 'NONE',  ( -14.61876137247786112, 180.8472868627314369, 317.6002088574783784 ) ) ;
#8926 = AXIS2_PLACEMENT_3D ( 'NONE', #19341, #5663, #10614 ) ;
#8927 = VERTEX_POINT ( 'NONE', #21509 ) ;
#8928 = CIRCLE ( 'NONE', #8208, 96.00000000000000000 ) ;
#8929 = CARTESIAN_POINT ( 'NONE',  ( 20.45030313596652860, 182.1143970192508164, 312.2990932916914630 ) ) ;
#8930 = EDGE_LOOP ( 'NONE', ( #10507, #7593, #10925, #987 ) ) ;
#8931 = B_SPLINE_CURVE_WITH_KNOTS ( 'NONE', 3,
 ( #17332, #19144, #8581, #15620, #6854, #16187, #6971, #13998, #5238, #12282, #19264, #10542, #17561, #1812, #18022, #16080 ),
 .UNSPECIFIED., .F., .F.,
 ( 4, 2, 2, 2, 2, 2, 2, 4 ),
 ( 0.000000000000000000, 0.0004291333152394312378, 0.0008582666304788624757, 0.001716533260957770054, 0.002145666576197221946, 0.002574799891436673621, 0.003003933206676125730, 0.003433066521915577405 ),
 .UNSPECIFIED. ) ;
#8932 = CARTESIAN_POINT ( 'NONE',  ( -39.42082737383935154, 91.17157287525387233, 83.51645567887779009 ) ) ;
#8933 = EDGE_CURVE ( 'NONE', #15010, #9718, #3611, .T. ) ;
#8934 = CARTESIAN_POINT ( 'NONE',  ( 35.92446336679496000, 93.51775827232349059, 82.02042234242476582 ) ) ;
#8935 = CIRCLE ( 'NONE', #5249, 10.00000000000000888 ) ;
#8936 = DIRECTION ( 'NONE',  ( 0.01292414190464178173, 1.902755938799531414E-22, 0.9999164797902017066 ) ) ;
#8937 = EDGE_CURVE ( 'NONE', #14770, #7130, #5777, .T. ) ;
#8938 = CARTESIAN_POINT ( 'NONE',  ( 51.18612362345588451, 111.9218655255083235, -48.12006336945275820 ) ) ;
#8939 = VECTOR ( 'NONE', #20208, 999.9999999999998863 ) ;
#8940 = DIRECTION ( 'NONE',  ( 0.009760756503428037745, -0.9999378516499566327, 0.005387065077611006073 ) ) ;
#8941 = LINE ( 'NONE', #21122, #10275 ) ;
#8942 = ORIENTED_EDGE ( 'NONE', *, *, #3252, .F. ) ;
#8943 = CYLINDRICAL_SURFACE ( 'NONE', #12110, 2.009999999999996678 ) ;
#8944 = ORIENTED_EDGE ( 'NONE', *, *, #20919, .T. ) ;
#8945 =( NAMED_UNIT ( * ) SI_UNIT ( $, .STERADIAN. ) SOLID_ANGLE_UNIT ( ) );
#8946 = DIRECTION ( 'NONE',  ( 0.3101392564284308762, 0.9506461370142480494, -0.009250070373106863975 ) ) ;
#8947 = CARTESIAN_POINT ( 'NONE',  ( -41.47069032946998846, 166.0668615304125808, 273.1833561390217824 ) ) ;
#8948 = FACE_BOUND ( 'NONE', #1587, .T. ) ;
#8949 = APPLICATION_CONTEXT ( 'automotive_design' ) ;
#8950 = EDGE_CURVE ( 'NONE', #8624, #16665, #19784, .T. ) ;
#8951 = ORIENTED_EDGE ( 'NONE', *, *, #6650, .F. ) ;
#8952 = DIRECTION ( 'NONE',  ( 7.125109674161246868E-05, -0.9999848031710253382, 0.005512562950850155054 ) ) ;
#8953 = CARTESIAN_POINT ( 'NONE',  ( 38.69757710431291287, 94.02752048664899576, 82.47923521851859618 ) ) ;
#8954 = AXIS2_PLACEMENT_3D ( 'NONE', #8703, #17236, #7119 ) ;
#8955 = CARTESIAN_POINT ( 'NONE',  ( -0.1034336282460315837, 327.3082181160931441, 316.1934087155942166 ) ) ;
#8956 = ORIENTED_EDGE ( 'NONE', *, *, #12924, .T. ) ;
#8957 = CIRCLE ( 'NONE', #21777, 1.999999999999997558 ) ;
#8958 = CIRCLE ( 'NONE', #18870, 7.921742784567028295 ) ;
#8959 = DIRECTION ( 'NONE',  ( 0.01292394549866739996, 0.005513023399720822122, 0.9999012842304692006 ) ) ;
#8960 = CARTESIAN_POINT ( 'NONE',  ( -90.09360468281239775, 87.50216161139763926, 51.09253514669736518 ) ) ;
#8961 = EDGE_LOOP ( 'NONE', ( #19330, #4244, #12826, #16318 ) ) ;
#8962 = ADVANCED_FACE ( 'NONE', ( #5331 ), #15818, .T. ) ;
#8963 = VERTEX_POINT ( 'NONE', #10521 ) ;
#8964 = DIRECTION ( 'NONE',  ( -2.025474946048326393E-22, 1.000000000000000000, -1.876735158486679873E-22 ) ) ;
#8965 =( BOUNDED_CURVE ( )  B_SPLINE_CURVE ( 3, ( #19642, #11161, #16580, #16697 ),
 .UNSPECIFIED., .F., .T. ) 
 B_SPLINE_CURVE_WITH_KNOTS ( ( 4, 4 ),
 ( 0.4229686233981270749, 0.4841788640348455575 ),
 .UNSPECIFIED. ) 
 CURVE ( )  GEOMETRIC_REPRESENTATION_ITEM ( )  RATIONAL_B_SPLINE_CURVE ( ( 1.000000000000000000, 0.9996877999070342691, 0.9996877999070342691, 1.000000000000000000 ) ) 
 REPRESENTATION_ITEM ( '' )  );
#8966 = FACE_OUTER_BOUND ( 'NONE', #18599, .T. ) ;
#8967 = CIRCLE ( 'NONE', #5670, 1.999999999999999112 ) ;
#8968 = CARTESIAN_POINT ( 'NONE',  ( 81.38158604529294848, 75.12830914639056346, 3.884784555313749888 ) ) ;
#8969 = CARTESIAN_POINT ( 'NONE',  ( -64.98109895693632154, 170.8565945647193587, 1.882390201297356347 ) ) ;
#8970 = ORIENTED_EDGE ( 'NONE', *, *, #17846, .T. ) ;
#8971 = CARTESIAN_POINT ( 'NONE',  ( 91.27111462898963623, 78.10400798472784345, 30.35002675991152898 ) ) ;
#8972 = ORIENTED_EDGE ( 'NONE', *, *, #22556, .T. ) ;
#8973 = FACE_OUTER_BOUND ( 'NONE', #4269, .T. ) ;
#8974 = LINE ( 'NONE', #8730, #14097 ) ;
#8975 = CARTESIAN_POINT ( 'NONE',  ( -44.65237404513518271, 168.6466622724118452, 27.18596972279685531 ) ) ;
#8976 = CARTESIAN_POINT ( 'NONE',  ( -13.33655421047878953, 164.7550532780195454, 317.2606976044711473 ) ) ;
#8977 = ORIENTED_EDGE ( 'NONE', *, *, #21764, .F. ) ;
#8978 = CARTESIAN_POINT ( 'NONE',  ( -55.33623483430230294, 88.81971041278778500, 167.7780138627090025 ) ) ;
#8979 = EDGE_CURVE ( 'NONE', #3953, #15318, #10861, .T. ) ;
#8980 = ORIENTED_EDGE ( 'NONE', *, *, #11755, .T. ) ;
#8981 = CARTESIAN_POINT ( 'NONE',  ( -91.23603883849614249, 72.00000000000000000, -30.82342686631250217 ) ) ;
#8982 = DIRECTION ( 'NONE',  ( 7.125109674364534776E-05, -0.9999848031710252272, 0.005512562950849704893 ) ) ;
#8983 = DIRECTION ( 'NONE',  ( 0.009760756503428004785, -0.9999378516499564107, 0.005387065077611765014 ) ) ;
#8984 = ORIENTED_EDGE ( 'NONE', *, *, #8479, .T. ) ;
#8985 = CARTESIAN_POINT ( 'NONE',  ( 41.56623493000984126, 91.17157287525387233, 82.46967996629570052 ) ) ;
#8986 = EDGE_LOOP ( 'NONE', ( #21163, #21866, #10225 ) ) ;
#8987 = AXIS2_PLACEMENT_3D ( 'NONE', #843, #6556, #8176 ) ;
#8988 = VERTEX_POINT ( 'NONE', #8895 ) ;
#8989 = UNCERTAINTY_MEASURE_WITH_UNIT (LENGTH_MEASURE( 1.000000000000000082E-05 ), #1870, 'distance_accuracy_value', 'NONE');
#8990 = CARTESIAN_POINT ( 'NONE',  ( 19.88292633637799156, 183.6120083857789780, 315.1481641239921032 ) ) ;
#8991 = VERTEX_POINT ( 'NONE', #12594 ) ;
#8992 = EDGE_CURVE ( 'NONE', #17081, #19439, #19351, .T. ) ;
#8993 = CARTESIAN_POINT ( 'NONE',  ( 47.39680884166017449, 144.7440243326373945, -46.97795445436837980 ) ) ;
#8994 = EDGE_CURVE ( 'NONE', #12945, #18985, #6983, .T. ) ;
#8995 = DIRECTION ( 'NONE',  ( -0.9934404589540162256, -0.1135548637187059617, 0.01346653032743144220 ) ) ;
#8996 = CARTESIAN_POINT ( 'NONE',  ( -2.673171722481940016, 142.9732003400563656, 275.3325226564539889 ) ) ;
#8997 = FACE_OUTER_BOUND ( 'NONE', #7617, .T. ) ;
#8998 = FACE_OUTER_BOUND ( 'NONE', #15035, .T. ) ;
#8999 = FACE_OUTER_BOUND ( 'NONE', #3443, .T. ) ;
#9000 = CIRCLE ( 'NONE', #5337, 75.00000000000002842 ) ;
#9001 = CARTESIAN_POINT ( 'NONE',  ( 85.37691781808469216, 75.05100517808324412, -4.234898060786123963 ) ) ;
#9002 = CARTESIAN_POINT ( 'NONE',  ( 12.53471727977827044, 187.5120739667221699, 307.7020987390404230 ) ) ;
#9003 = CARTESIAN_POINT ( 'NONE',  ( 91.45164190239772495, 80.14421549785700449, 29.66212192225453848 ) ) ;
#9004 = DIRECTION ( 'NONE',  ( -0.01292394549866632963, -0.005513023399716958026, -0.9999012842304692006 ) ) ;
#9005 = SHAPE_REPRESENTATION_RELATIONSHIP ( 'NONE' , 'NONE' ,  #10182, #16783 ) ;
#9006 = DIRECTION ( 'NONE',  ( -0.9934404589540165587, -0.1135548637187045462, 0.01346653032743214476 ) ) ;
#9007 = CARTESIAN_POINT ( 'NONE',  ( -42.64951291394369548, 126.1473081376431367, 27.39440536439884255 ) ) ;
#9008 = EDGE_LOOP ( 'NONE', ( #20921, #10690 ) ) ;
#9009 = CARTESIAN_POINT ( 'NONE',  ( -91.87497954589036908, 77.44324451750601668, -29.32612497091890802 ) ) ;
#9010 = ORIENTED_EDGE ( 'NONE', *, *, #12797, .T. ) ;
#9011 = CONICAL_SURFACE ( 'NONE', #6084, 6.000000000000000888, 0.7853981633974509435 ) ;
#9012 = PRODUCT_DEFINITION_SHAPE ( 'NONE', 'NONE',  #22689 ) ;
#9013 = LINE ( 'NONE', #3855, #1500 ) ;
#9014 = DIRECTION ( 'NONE',  ( -7.125109674243555432E-05, 0.9999848031710253382, -0.005512562950850175003 ) ) ;
#9015 = PLANE ( 'NONE',  #1403 ) ;
#9016 = DIRECTION ( 'NONE',  ( -0.01292394549866741384, -0.005513023399720269613, -0.9999012842304692006 ) ) ;
#9017 = ORIENTED_EDGE ( 'NONE', *, *, #14235, .F. ) ;
#9018 = DIRECTION ( 'NONE',  ( 0.01292394549866728373, 0.005513023399720296501, 0.9999012842304693116 ) ) ;
#9019 = EDGE_LOOP ( 'NONE', ( #11188, #8480, #9161, #2331 ) ) ;
#9020 = CARTESIAN_POINT ( 'NONE',  ( 80.05923150692980528, 75.13699351169597662, 4.065642694558706083 ) ) ;
#9021 = DIRECTION ( 'NONE',  ( -0.9999164797902017066, -2.001050586450178931E-22, 0.01292414190464131508 ) ) ;
#9022 = SURFACE_STYLE_USAGE ( .BOTH. , #19695 ) ;
#9023 = CARTESIAN_POINT ( 'NONE',  ( -90.65029634199436259, 79.17021053268413766, 29.01211804384233517 ) ) ;
#9024 = CARTESIAN_POINT ( 'NONE',  ( -163.1715728752537871, 20.00000000000000000, -8.828427124746170307 ) ) ;
#9025 = ORIENTED_EDGE ( 'NONE', *, *, #21950, .F. ) ;
#9026 = CARTESIAN_POINT ( 'NONE',  ( -14.73958462865978980, 180.7047163397708971, 312.0297913800017113 ) ) ;
#9027 = DIRECTION ( 'NONE',  ( 0.9909299940865190504, -0.1338359446631136318, -0.01207007604876911971 ) ) ;
#9028 = CARTESIAN_POINT ( 'NONE',  ( 5.986268468634207807, 81.99999999999998579, -84.52572088931836447 ) ) ;
#9029 = CARTESIAN_POINT ( 'NONE',  ( -13.46575745744828367, 183.1864814975198215, 319.4298558866661324 ) ) ;
#9030 = CARTESIAN_POINT ( 'NONE',  ( 41.56623493000984126, 72.00000000000000000, 82.46967996629570052 ) ) ;
#9031 = PLANE ( 'NONE',  #9242 ) ;
#9032 = CONTEXT_DEPENDENT_SHAPE_REPRESENTATION ( #20988, #13608 ) ;
#9033 = EDGE_CURVE ( 'NONE', #15210, #18024, #5889, .T. ) ;
#9034 = EDGE_CURVE ( 'NONE', #4443, #13282, #19462, .T. ) ;
#9035 = DIRECTION ( 'NONE',  ( 0.000000000000000000, 0.000000000000000000, 1.000000000000000000 ) ) ;
#9036 = CARTESIAN_POINT ( 'NONE',  ( -17.11750112564732618, 315.9920795429054010, 328.5475409320285962 ) ) ;
#9037 = CARTESIAN_POINT ( 'NONE',  ( 39.42082737383939417, 91.17157287525388654, -83.51645567887783272 ) ) ;
#9038 = VERTEX_POINT ( 'NONE', #525 ) ;
#9039 = ORIENTED_EDGE ( 'NONE', *, *, #8086, .F. ) ;
#9040 = CARTESIAN_POINT ( 'NONE',  ( 88.24077620913463704, 100.2813628572214384, -65.67913105001751717 ) ) ;
#9041 = DIRECTION ( 'NONE',  ( -0.01292394549866632963, -0.005513023399716958026, -0.9999012842304692006 ) ) ;
#9042 = ORIENTED_EDGE ( 'NONE', *, *, #6130, .F. ) ;
#9043 = CARTESIAN_POINT ( 'NONE',  ( -42.64951291394369548, 126.1473081376431367, 27.39440536439884255 ) ) ;
#9044 = VERTEX_POINT ( 'NONE', #11425 ) ;
#9045 = CARTESIAN_POINT ( 'NONE',  ( -9.034450215842609211, 187.2654037237712146, 277.6052983116423434 ) ) ;
#9046 = DIRECTION ( 'NONE',  ( -0.01292394549866741384, -0.005513023399720269613, -0.9999012842304692006 ) ) ;
#9047 = DIRECTION ( 'NONE',  ( 0.01035335185279143318, 0.005513005182356926943, 0.9999312050732649393 ) ) ;
#9048 = CARTESIAN_POINT ( 'NONE',  ( 51.71043826665287924, 166.8507685304810764, 255.9730676870379114 ) ) ;
#9049 = ADVANCED_FACE ( 'NONE', ( #4061 ), #20125, .F. ) ;
#9050 = ORIENTED_EDGE ( 'NONE', *, *, #12293, .T. ) ;
#9051 = CARTESIAN_POINT ( 'NONE',  ( 9.196690372329049623, 142.8086146031528187, 274.7267082784170498 ) ) ;
#9052 = CONICAL_SURFACE ( 'NONE', #17903, 2.499999999999988010, 1.029744258676651425 ) ;
#9053 = CARTESIAN_POINT ( 'NONE',  ( -11.23547344339351284, 137.5384677217048193, 97.91481361337272915 ) ) ;
#9054 = ADVANCED_FACE ( 'NONE', ( #21951 ), #7965, .T. ) ;
#9055 = CARTESIAN_POINT ( 'NONE',  ( 20.69463332847445614, 186.0431207901125674, 276.2701100107056504 ) ) ;
#9056 = VERTEX_POINT ( 'NONE', #6137 ) ;
#9057 = B_SPLINE_CURVE_WITH_KNOTS ( 'NONE', 3,
 ( #6121, #16610, #20113, #2344, #9345, #17878, #7388, #14432, #16382, #7615, #14654, #19897, #4167, #11194, #18422, #13711, #16937, #1315 ),
 .UNSPECIFIED., .F., .F.,
 ( 4, 2, 2, 2, 2, 2, 2, 2, 4 ),
 ( 0.000000000000000000, 0.0008023074076923488894, 0.001604614815384697779, 0.002406922223077046560, 0.003209229630769395557, 0.004011537038461744122, 0.004813844446154093119, 0.005616151853846442117, 0.006418459261538791115 ),
 .UNSPECIFIED. ) ;
#9058 = CARTESIAN_POINT ( 'NONE',  ( -54.52327687265817246, 18.00000000000000355, -111.3697098814011781 ) ) ;
#9059 = CARTESIAN_POINT ( 'NONE',  ( -88.16590590355198742, 88.48929759811795748, 52.69915227853057615 ) ) ;
#9060 = APPLICATION_PROTOCOL_DEFINITION ( 'draft international standard', 'automotive_design', 1998, #8506 ) ;
#9061 = EDGE_CURVE ( 'NONE', #14836, #3481, #5519, .T. ) ;
#9062 = ORIENTED_EDGE ( 'NONE', *, *, #14777, .F. ) ;
#9063 = EDGE_CURVE ( 'NONE', #345, #5676, #14364, .T. ) ;
#9064 = VERTEX_POINT ( 'NONE', #1090 ) ;
#9065 = CARTESIAN_POINT ( 'NONE',  ( -14.53239793090661180, 175.6255473142593644, 113.6490011371711688 ) ) ;
#9066 = DIRECTION ( 'NONE',  ( -0.004263634442766563518, -0.9440169652124856814, -0.3298693541575922761 ) ) ;
#9067 = EDGE_CURVE ( 'NONE', #12198, #3438, #11407, .T. ) ;
#9068 = FACE_OUTER_BOUND ( 'NONE', #13927, .T. ) ;
#9069 = FACE_OUTER_BOUND ( 'NONE', #18144, .T. ) ;
#9070 = CONICAL_SURFACE ( 'NONE', #13141, 4.999999999999997335, 0.7853981633974496113 ) ;
#9071 = CARTESIAN_POINT ( 'NONE',  ( -1.163172771417702700, 69.99999999999998579, -89.99248318111824574 ) ) ;
#9072 = ORIENTED_EDGE ( 'NONE', *, *, #22132, .F. ) ;
#9074 = CARTESIAN_POINT ( 'NONE',  ( 92.91906646248270363, 77.13883058002313931, 28.81763569833105976 ) ) ;
#9073 = B_SPLINE_CURVE_WITH_KNOTS ( 'NONE', 3,
 ( #17191, #16993, #11463, #4887, #15709, #8900, #14102, #3619, #20743, #71, #17785, #10630, #17541, #17433 ),
 .UNSPECIFIED., .F., .F.,
 ( 4, 2, 2, 2, 2, 2, 4 ),
 ( 0.000000000000000000, 0.0005169893790259204921, 0.001033978758051840984, 0.001550968137077761476, 0.002067957516103681968, 0.003101936274155522952, 0.004135915032207363937 ),
 .UNSPECIFIED. ) ;
#9075 = VERTEX_POINT ( 'NONE', #13062 ) ;
#9076 = DIRECTION ( 'NONE',  ( -0.9235411807339423129, -0.002179866145371284376, -0.3834930712179088763 ) ) ;
#9077 = AXIS2_PLACEMENT_3D ( 'NONE', #17896, #12720, #15832 ) ;
#9078 = CARTESIAN_POINT ( 'NONE',  ( 4.306364041547309895, 81.44153265534502850, -98.35747069930887676 ) ) ;
#9079 = DIRECTION ( 'NONE',  ( -0.9999164797902017066, -6.965998958219367529E-18, 0.01292414190464157182 ) ) ;
#9080 = CARTESIAN_POINT ( 'NONE',  ( -9.069298571189188252, 165.2074204917897475, 308.4306052290647813 ) ) ;
#9081 = DIRECTION ( 'NONE',  ( -2.025474946048326158E-22, 1.000000000000000000, -1.876735158486679638E-22 ) ) ;
#9082 = CARTESIAN_POINT ( 'NONE',  ( -40.07458683857907289, 107.0042576524874818, 71.63327710005648896 ) ) ;
#9083 = LINE ( 'NONE', #16371, #4570 ) ;
#9084 = CARTESIAN_POINT ( 'NONE',  ( 105.1274178938603825, 70.25451017443431567, -32.37651503794369034 ) ) ;
#9085 = AXIS2_PLACEMENT_3D ( 'NONE', #12787, #13249, #7500 ) ;
#9086 = ORIENTED_EDGE ( 'NONE', *, *, #1139, .T. ) ;
#9087 = ADVANCED_FACE ( 'NONE', ( #7624 ), #19084, .F. ) ;
#9088 = DIRECTION ( 'NONE',  ( -5.440186201345738641E-18, -1.000000000000000000, -1.334940939666364181E-17 ) ) ;
#9089 = ORIENTED_EDGE ( 'NONE', *, *, #6844, .T. ) ;
#9090 = EDGE_LOOP ( 'NONE', ( #4027, #11947, #2704 ) ) ;
#9091 = EDGE_LOOP ( 'NONE', ( #4356, #15782, #7793, #6125 ) ) ;
#9092 = CARTESIAN_POINT ( 'NONE',  ( -83.78835501158950194, 75.05963785504690122, 4.457120374836909704 ) ) ;
#9093 = CONICAL_SURFACE ( 'NONE', #10207, 6.000000000000000888, 0.9599310885968777018 ) ;
#9094 = CARTESIAN_POINT ( 'NONE',  ( 18.45279573939507145, 185.6574623812839491, 318.1353495108407969 ) ) ;
#9095 =( BOUNDED_SURFACE ( )  B_SPLINE_SURFACE ( 3, 2, ( 
 ( #20739, #4990, #12018 ),
 ( #19006, #3268, #1570 ),
 ( #22543, #6836, #19121 ),
 ( #3398, #5217, #19354 ),
 ( #12711, #17657, #3733 ),
 ( #17780, #20959, #21299 ),
 ( #10752, #19678, #16291 ),
 ( #1788, #15822, #12479 ),
 ( #19465, #21079, #10969 ),
 ( #9009, #19243, #3508 ),
 ( #5335, #8769, #3947 ),
 ( #2021, #21412, #13968 ),
 ( #14098, #12597, #12373 ),
 ( #10524, #17997, #17538 ),
 ( #188, #10626, #1906 ),
 ( #3614, #5565, #412 ),
 ( #2236, #15946, #67 ),
 ( #12254, #14451, #7067 ) ),
 .UNSPECIFIED., .F., .F., .T. ) 
 B_SPLINE_SURFACE_WITH_KNOTS ( ( 4, 2, 2, 2, 2, 2, 2, 2, 4 ),
 ( 3, 3 ),
 ( 0.003005090483489989556, 0.003807341501471057498, 0.004609592519452125441, 0.005411843537433192949, 0.006214094555414261326, 0.007016345573395328834, 0.007818596591376396343, 0.008620847609357464719, 0.009423098627338533095 ),
 ( 0.000000000000000000, 1.000000000000000000 ),
 .UNSPECIFIED. ) 
 GEOMETRIC_REPRESENTATION_ITEM ( )  RATIONAL_B_SPLINE_SURFACE ( (
 ( 1.000000000000000000, 0.7071067811865485719, 1.000000000000000000),
 ( 1.000000000000000000, 0.6996407321460798023, 1.000000000000000000),
 ( 1.000000000000000000, 0.6923367522676026065, 1.000000000000000000),
 ( 1.000000000000000000, 0.6780525511373404202, 1.000000000000000000),
 ( 1.000000000000000000, 0.6710180578259783424, 1.000000000000000000),
 ( 1.000000000000000000, 0.6575437683257994159, 1.000000000000000000),
 ( 1.000000000000000000, 0.6511910073847769764, 1.000000000000000000),
 ( 1.000000000000000000, 0.6392329869082821192, 1.000000000000000000),
 ( 1.000000000000000000, 0.6335699185532992495, 1.000000000000000000),
 ( 1.000000000000000000, 0.6233860397584745083, 1.000000000000000000),
 ( 1.000000000000000000, 0.6188536248677669604, 1.000000000000000000),
 ( 1.000000000000000000, 0.6108845495338486309, 1.000000000000000000),
 ( 1.000000000000000000, 0.6074396204518894837, 1.000000000000000000),
 ( 1.000000000000000000, 0.6019717515916982453, 1.000000000000000000),
 ( 1.000000000000000000, 0.5998961748958268059, 1.000000000000000000),
 ( 1.000000000000000000, 0.5970819659646876554, 1.000000000000000000),
 ( 1.000000000000000000, 0.5963755918899067421, 1.000000000000000000),
 ( 1.000000000000000000, 0.5963808372950819559, 1.000000000000000000) ) ) 
 REPRESENTATION_ITEM ( '' )  SURFACE ( )  );
#9097 = EDGE_LOOP ( 'NONE', ( #19053, #8700, #20878, #18030, #947 ) ) ;
#9096 = ORIENTED_EDGE ( 'NONE', *, *, #1509, .T. ) ;
#9098 = EDGE_CURVE ( 'NONE', #13090, #16716, #22391, .T. ) ;
#9099 = DIRECTION ( 'NONE',  ( -0.01292394549866740690, -0.005513023399721241925, -0.9999012842304693116 ) ) ;
#9100 = DIRECTION ( 'NONE',  ( -0.9726991065672926373, -0.2316562896908763991, 0.01384960395994897994 ) ) ;
#9101 = LINE ( 'NONE', #8881, #13189 ) ;
#9102 = VECTOR ( 'NONE', #7529, 1000.000000000000114 ) ;
#9103 = CARTESIAN_POINT ( 'NONE',  ( -38.79722561300751238, 125.3640259171584290, 248.0640311032106524 ) ) ;
#9104 = CARTESIAN_POINT ( 'NONE',  ( -38.22145853964982365, 96.26286894743961398, 84.82045450040972412 ) ) ;
#9105 = CIRCLE ( 'NONE', #12058, 7.499999999999991118 ) ;
#9106 = COLOUR_RGB ( '', 0.08235294, 0.09019608, 0.10196078) ;
#9107 = CARTESIAN_POINT ( 'NONE',  ( 13.04687021101641342, 190.3009381008880609, 320.8498765639175190 ) ) ;
#9108 = DIRECTION ( 'NONE',  ( -0.1136178953597575675, 0.9935164314186356593, -0.004009283626633515681 ) ) ;
#9109 = CARTESIAN_POINT ( 'NONE',  ( 14.60385163837487532, 186.5550067726685484, 307.9188285726191339 ) ) ;
#9110 = B_SPLINE_CURVE_WITH_KNOTS ( 'NONE', 3,
 ( #8734, #5648, #7038, #17088, #21049, #15789, #17507, #3585 ),
 .UNSPECIFIED., .F., .F.,
 ( 4, 2, 2, 4 ),
 ( 4.486197489951441732E-16, 0.0007139082715502006972, 0.001427816543099952751, 0.002855633086199477026 ),
 .UNSPECIFIED. ) ;
#9111 = CARTESIAN_POINT ( 'NONE',  ( 89.22443767324084263, 80.23075532867255788, 29.93879111800735870 ) ) ;
#9112 = CARTESIAN_POINT ( 'NONE',  ( 89.22767861003025303, 80.31838830481380853, 30.18953644180655971 ) ) ;
#9113 = ORIENTED_EDGE ( 'NONE', *, *, #17226, .T. ) ;
#9114 =( NAMED_UNIT ( * ) PLANE_ANGLE_UNIT ( ) SI_UNIT ( $, .RADIAN. ) );
#9115 = EDGE_CURVE ( 'NONE', #11327, #20863, #790, .T. ) ;
#9116 = CARTESIAN_POINT ( 'NONE',  ( -8.943793367660859417, 186.3714091404604858, 321.6764070892438099 ) ) ;
#9117 = DIRECTION ( 'NONE',  ( 0.000000000000000000, -0.000000000000000000, 1.000000000000000000 ) ) ;
#9118 = ADVANCED_FACE ( 'NONE', ( #14786 ), #12941, .T. ) ;
#9119 = VERTEX_POINT ( 'NONE', #14665 ) ;
#9120 = DIRECTION ( 'NONE',  ( 7.125109674161246868E-05, -0.9999848031710252272, 0.005512562950850154186 ) ) ;
#9121 = EDGE_LOOP ( 'NONE', ( #19201, #4156, #9793, #9745 ) ) ;
#9122 = VECTOR ( 'NONE', #16689, 1000.000000000000227 ) ;
#9123 = ORIENTED_EDGE ( 'NONE', *, *, #12387, .T. ) ;
#9124 = CIRCLE ( 'NONE', #20134, 2.499999999999988010 ) ;
#9125 = ORIENTED_EDGE ( 'NONE', *, *, #19887, .T. ) ;
#9126 = CARTESIAN_POINT ( 'NONE',  ( -38.63447605617402303, 163.9374297322429470, 277.1588331099309812 ) ) ;
#9127 = ORIENTED_EDGE ( 'NONE', *, *, #12004, .F. ) ;
#9128 = DIRECTION ( 'NONE',  ( 0.9999164797902015955, 6.965998958219364448E-18, -0.01292414190464157182 ) ) ;
#9129 = CARTESIAN_POINT ( 'NONE',  ( 85.09289243014617909, 54.99999999999999289, -1.099844476084985700 ) ) ;
#9130 = DIRECTION ( 'NONE',  ( 0.01292414190464131335, 1.902755938799530239E-22, 0.9999164797902015955 ) ) ;
#9131 = VERTEX_POINT ( 'NONE', #6026 ) ;
#9132 = CARTESIAN_POINT ( 'NONE',  ( 12.13657183616750679, 187.7271216158292759, 322.9769951237993268 ) ) ;
#9133 = CLOSED_SHELL ( 'NONE', ( #1624, #10629, #2475, #1359, #378, #12287, #7509, #21761 ) ) ;
#9134 = VERTEX_POINT ( 'NONE', #2465 ) ;
#9135 = EDGE_LOOP ( 'NONE', ( #1005, #21061, #9355, #6235 ) ) ;
#9136 = CARTESIAN_POINT ( 'NONE',  ( 10.15309714582121714, 176.0218267656414355, 323.4662548820142547 ) ) ;
#9137 = CIRCLE ( 'NONE', #1455, 3.047499999999988329 ) ;
#9138 = CARTESIAN_POINT ( 'NONE',  ( 50.94927467532792775, 107.7466302394140172, 69.13694936332524321 ) ) ;
#9139 = CARTESIAN_POINT ( 'NONE',  ( -9.258875922456445196, 185.4416665633954153, 321.2584118180014912 ) ) ;
#9140 = CARTESIAN_POINT ( 'NONE',  ( -91.40469917791146770, 79.08369667522879354, 28.73783386972080223 ) ) ;
#9141 = DIRECTION ( 'NONE',  ( -0.01104128644981183967, -0.5197558313507629757, -0.8542435049623791077 ) ) ;
#9142 = ORIENTED_EDGE ( 'NONE', *, *, #20661, .F. ) ;
#9143 = CARTESIAN_POINT ( 'NONE',  ( -13.95813346672372468, 182.2598320623498580, 318.8173946239458587 ) ) ;
#9144 = ORIENTED_EDGE ( 'NONE', *, *, #2229, .F. ) ;
#9145 = EDGE_CURVE ( 'NONE', #3099, #10294, #4397, .T. ) ;
#9146 = CARTESIAN_POINT ( 'NONE',  ( 43.19592572978904599, 125.3640259171584290, 247.0042514670300591 ) ) ;
#9147 = LINE ( 'NONE', #12396, #13575 ) ;
#9148 = CARTESIAN_POINT ( 'NONE',  ( -12.86560286818836474, 181.5419395642671248, 319.9155313192819108 ) ) ;
#9149 = ORIENTED_EDGE ( 'NONE', *, *, #10055, .F. ) ;
#9150 = FACE_OUTER_BOUND ( 'NONE', #20714, .T. ) ;
#9151 = ORIENTED_EDGE ( 'NONE', *, *, #13317, .T. ) ;
#9152 = AXIS2_PLACEMENT_3D ( 'NONE', #230, #12523, #10677 ) ;
#9153 = AXIS2_PLACEMENT_3D ( 'NONE', #18636, #2797, #2897 ) ;
#9154 = CARTESIAN_POINT ( 'NONE',  ( 12.20664162007220099, 188.8323198333426376, 307.2129386106284983 ) ) ;
#9155 = CONTEXT_DEPENDENT_SHAPE_REPRESENTATION ( #13958, #17660 ) ;
#9156 = VECTOR ( 'NONE', #10687, 1000.000000000000227 ) ;
#9157 = PRODUCT_DEFINITION ( 'UNKNOWN', '', #21273, #12717 ) ;
#9158 = LINE ( 'NONE', #3981, #18804 ) ;
#9159 = CIRCLE ( 'NONE', #14347, 7.499999999999992006 ) ;
#9160 = CARTESIAN_POINT ( 'NONE',  ( -1.182511287347259854, 144.6672920925655319, 276.7810053806090309 ) ) ;
#9161 = ORIENTED_EDGE ( 'NONE', *, *, #1358, .F. ) ;
#9162 = DIRECTION ( 'NONE',  ( -0.01246513159389404414, -0.2641402835564772844, -0.9644037178988117409 ) ) ;
#9163 = CARTESIAN_POINT ( 'NONE',  ( -50.40543294395669704, 95.70122931221760609, -44.61497156429899746 ) ) ;
#9164 = EDGE_LOOP ( 'NONE', ( #7110, #90, #3636, #11129 ) ) ;
#9165 = DIRECTION ( 'NONE',  ( -0.01292394549866734098, -0.005513023399720419666, -0.9999012842304692006 ) ) ;
#9166 = LINE ( 'NONE', #7333, #22502 ) ;
#9167 = DIRECTION ( 'NONE',  ( 0.8981428216242073326, 1.525529167390024815E-15, 0.4397038457472340900 ) ) ;
#9168 = CARTESIAN_POINT ( 'NONE',  ( 7.165475679525708408, 86.29954751296186544, 75.08469730518739027 ) ) ;
#9169 = AXIS2_PLACEMENT_3D ( 'NONE', #12808, #9710, #16620 ) ;
#9170 = VECTOR ( 'NONE', #16724, 1000.000000000000000 ) ;
#9171 = CARTESIAN_POINT ( 'NONE',  ( -10.85608148985439492, 111.4593827568422171, 127.2676533951182307 ) ) ;
#9172 = PRODUCT_DEFINITION_FORMATION_WITH_SPECIFIED_SOURCE ( 'ANY', '', #7702, .NOT_KNOWN. ) ;
#9173 = ADVANCED_FACE ( 'NONE', ( #9712 ), #13275, .F. ) ;
#9174 = LINE ( 'NONE', #12759, #10270 ) ;
#9175 = VECTOR ( 'NONE', #17304, 1000.000000000000114 ) ;
#9176 = CIRCLE ( 'NONE', #3302, 2.499999999999988010 ) ;
#9177 = ORIENTED_EDGE ( 'NONE', *, *, #388, .F. ) ;
#9178 = LINE ( 'NONE', #12661, #10254 ) ;
#9179 = CARTESIAN_POINT ( 'NONE',  ( -88.96403593049780056, 88.58898090146213633, 50.41366170828801074 ) ) ;
#9180 = DIRECTION ( 'NONE',  ( -0.01356080911997353811, -0.01954840589401621309, -0.9997169420806143458 ) ) ;
#9181 = CIRCLE ( 'NONE', #17276, 10.00000000000000355 ) ;
#9182 = ORIENTED_EDGE ( 'NONE', *, *, #10898, .T. ) ;
#9183 = CIRCLE ( 'NONE', #6975, 24.23418050574097293 ) ;
#9184 = EDGE_CURVE ( 'NONE', #8189, #21685, #11546, .T. ) ;
#9185 = ORIENTED_EDGE ( 'NONE', *, *, #10277, .T. ) ;
#9186 = FACE_OUTER_BOUND ( 'NONE', #7361, .T. ) ;
#9187 = AXIS2_PLACEMENT_3D ( 'NONE', #2824, #8544, #4537 ) ;
#9188 = CARTESIAN_POINT ( 'NONE',  ( 1.143866695291850588, 165.4878681845327151, 88.49880848915942977 ) ) ;
#9189 = FILL_AREA_STYLE_COLOUR ( '', #17978 ) ;
#9190 = CARTESIAN_POINT ( 'NONE',  ( -106.2089377515398922, 71.86507807689916660, -28.62973177816246917 ) ) ;
#9191 = CARTESIAN_POINT ( 'NONE',  ( -91.51031840793912409, 96.48503848149375983, -61.03988419336481996 ) ) ;
#9192 = ORIENTED_EDGE ( 'NONE', *, *, #16690, .T. ) ;
#9193 = EDGE_CURVE ( 'NONE', #11275, #15988, #7381, .T. ) ;
#9194 = CARTESIAN_POINT ( 'NONE',  ( -63.99205529224568068, 99.43075776215394512, 78.40283286226222970 ) ) ;
#9195 = VECTOR ( 'NONE', #7086, 999.9999999999998863 ) ;
#9196 = VERTEX_POINT ( 'NONE', #7865 ) ;
#9197 = CARTESIAN_POINT ( 'NONE',  ( -41.41899454747532161, 166.0889136240114681, 277.1829612759436827 ) ) ;
#9198 = CARTESIAN_POINT ( 'NONE',  ( 1.143879619237349266, 165.4878736975560969, 88.49980839044366121 ) ) ;
#9199 = CARTESIAN_POINT ( 'NONE',  ( -75.89761971758728976, 75.05050884166004721, 4.091003432312519728 ) ) ;
#9200 = CARTESIAN_POINT ( 'NONE',  ( -7.685154071873219195, 165.4174906297564007, 321.2619620810605738 ) ) ;
#9201 = CARTESIAN_POINT ( 'NONE',  ( -88.07410310386867991, 72.00000000000001421, 59.83417019015373484 ) ) ;
#9202 = CYLINDRICAL_SURFACE ( 'NONE', #5964, 2.000000000000000000 ) ;
#9203 = CARTESIAN_POINT ( 'NONE',  ( 1.457329690985350156E-14, 25.00000000000000000, -118.0000000000000000 ) ) ;
#9204 = DIRECTION ( 'NONE',  ( 0.000000000000000000, 1.000000000000000000, -0.000000000000000000 ) ) ;
#9205 = EDGE_CURVE ( 'NONE', #2746, #7542, #9461, .T. ) ;
#9206 = ORIENTED_EDGE ( 'NONE', *, *, #12655, .T. ) ;
#9207 = EDGE_CURVE ( 'NONE', #12349, #134, #4439, .T. ) ;
#9208 = DIRECTION ( 'NONE',  ( 0.01292394549866637994, 0.005513023399719273882, 0.9999012842304692006 ) ) ;
#9209 = EDGE_CURVE ( 'NONE', #6936, #8421, #20211, .T. ) ;
#9210 = AXIS2_PLACEMENT_3D ( 'NONE', #16701, #20436, #948 ) ;
#9211 = VERTEX_POINT ( 'NONE', #4630 ) ;
#9212 = AXIS2_PLACEMENT_3D ( 'NONE', #22290, #6581, #3133 ) ;
#9213 = VERTEX_POINT ( 'NONE', #2913 ) ;
#9214 = TOROIDAL_SURFACE ( 'NONE', #2938, 83.00000000000001421, 2.000000000000000000 ) ;
#9215 = FACE_BOUND ( 'NONE', #20477, .T. ) ;
#9216 = VECTOR ( 'NONE', #6056, 999.9999999999998863 ) ;
#9218 = ORIENTED_EDGE ( 'NONE', *, *, #21109, .F. ) ;
#9217 = ORIENTED_EDGE ( 'NONE', *, *, #5108, .F. ) ;
#9219 = ADVANCED_FACE ( 'NONE', ( #16950 ), #1214, .T. ) ;
#9220 = CARTESIAN_POINT ( 'NONE',  ( 92.40872671617952960, 69.99999999999998579, -33.19707612406970298 ) ) ;
#9221 = DIRECTION ( 'NONE',  ( 0.9232306267972777425, 0.000000000000000000, -0.3842462878721220054 ) ) ;
#9222 = EDGE_CURVE ( 'NONE', #21883, #13585, #1152, .T. ) ;
#9223 = CARTESIAN_POINT ( 'NONE',  ( 7.145902869757795983, 69.99999999999998579, -93.45069977196735067 ) ) ;
#9224 = VECTOR ( 'NONE', #22621, 1000.000000000000000 ) ;
#9225 = CARTESIAN_POINT ( 'NONE',  ( 68.97076059960825489, 70.03291683438813209, 85.69217454375154830 ) ) ;
#9226 = EDGE_CURVE ( 'NONE', #15988, #7332, #13635, .T. ) ;
#9227 = AXIS2_PLACEMENT_3D ( 'NONE', #6374, #13395, #10382 ) ;
#9228 = LINE ( 'NONE', #11416, #11019 ) ;
#9229 = CARTESIAN_POINT ( 'NONE',  ( -92.40872671617950118, 72.00000000000000000, 33.19707612406966035 ) ) ;
#9230 = VECTOR ( 'NONE', #6202, 1000.000000000000114 ) ;
#9231 = CARTESIAN_POINT ( 'NONE',  ( 17.55321521090719727, 184.6409100556667795, 307.3691051642267666 ) ) ;
#9232 = CARTESIAN_POINT ( 'NONE',  ( 89.33542534687491354, 79.97945796766221349, 29.20190675877598352 ) ) ;
#9233 = DIRECTION ( 'NONE',  ( -0.01292414190464131335, 0.000000000000000000, -0.9999164797902017066 ) ) ;
#9234 = VECTOR ( 'NONE', #19742, 999.9999999999998863 ) ;
#9235 = ADVANCED_FACE ( 'NONE', ( #17801 ), #409, .T. ) ;
#9236 = DIRECTION ( 'NONE',  ( 7.125109674160258889E-05, -0.9999848031710252272, 0.005512562950849897447 ) ) ;
#9237 = FACE_OUTER_BOUND ( 'NONE', #4762, .T. ) ;
#9238 = ORIENTED_EDGE ( 'NONE', *, *, #2654, .F. ) ;
#9240 = CYLINDRICAL_SURFACE ( 'NONE', #20469, 6.499999999999998224 ) ;
#9239 = VECTOR ( 'NONE', #6040, 999.9999999999998863 ) ;
#9241 = ORIENTED_EDGE ( 'NONE', *, *, #2649, .T. ) ;
#9242 = AXIS2_PLACEMENT_3D ( 'NONE', #21110, #14006, #5134 ) ;
#9243 = VECTOR ( 'NONE', #2166, 1000.000000000000000 ) ;
#9244 = CYLINDRICAL_SURFACE ( 'NONE', #2743, 110.5324305509042233 ) ;
#9245 = CARTESIAN_POINT ( 'NONE',  ( -7.243839870924983160, 81.92338897118676755, -96.85699015411138646 ) ) ;
#9246 = AXIS2_PLACEMENT_3D ( 'NONE', #5027, #13558, #20884 ) ;
#9247 = CARTESIAN_POINT ( 'NONE',  ( 74.91776319474617196, 75.00176710950381676, -1.633185153038630100 ) ) ;
#9248 = DIRECTION ( 'NONE',  ( 0.01292394549866740169, 0.005513023399720822990, 0.9999012842304693116 ) ) ;
#9249 = CARTESIAN_POINT ( 'NONE',  ( 68.30941429790007646, 191.4143309225247549, 255.6230893828509352 ) ) ;
#9250 = CARTESIAN_POINT ( 'NONE',  ( 77.86064527566928462, 75.18028080999435758, 4.844510309476128818 ) ) ;
#9251 = CARTESIAN_POINT ( 'NONE',  ( 1.364373935098378649E-14, 105.0000000000000000, -9.836450281572198869E-15 ) ) ;
#9252 = DIRECTION ( 'NONE',  ( -0.9250486434174662875, -0.3795887553195633202, 0.01404934683357507604 ) ) ;
#9253 = EDGE_CURVE ( 'NONE', #6890, #11929, #19369, .T. ) ;
#9254 = ORIENTED_EDGE ( 'NONE', *, *, #16389, .T. ) ;
#9255 = ORIENTED_EDGE ( 'NONE', *, *, #21675, .F. ) ;
#9256 = DIRECTION ( 'NONE',  ( 0.2065246940633230777, -0.0001041297050211054120, 0.9784413829653033634 ) ) ;
#9257 = CIRCLE ( 'NONE', #5581, 110.0000000000000000 ) ;
#9258 = CARTESIAN_POINT ( 'NONE',  ( 93.18417523045800976, 77.12912189496647386, 26.79791266334236610 ) ) ;
#9259 = AXIS2_PLACEMENT_3D ( 'NONE', #13082, #1002, #14810 ) ;
#9260 = DIRECTION ( 'NONE',  ( 7.125109674160325297E-05, -0.9999848031710253382, 0.005512562950849327591 ) ) ;
#9261 = LINE ( 'NONE', #16310, #18774 ) ;
#9262 = CARTESIAN_POINT ( 'NONE',  ( -91.76144944056422048, 79.85812038788782274, 31.26012496009715846 ) ) ;
#9263 = CARTESIAN_POINT ( 'NONE',  ( -164.0000000000000284, 19.17157287525381193, -7.999999999999978684 ) ) ;
#9264 = ORIENTED_EDGE ( 'NONE', *, *, #743, .T. ) ;
#9265 = DIRECTION ( 'NONE',  ( -0.009760756503428008254, 0.9999378516499565217, -0.005387065077611300108 ) ) ;
#9266 = EDGE_LOOP ( 'NONE', ( #18337, #6658, #17075, #15334 ) ) ;
#9267 = ADVANCED_FACE ( 'NONE', ( #14470 ), #10539, .F. ) ;
#9268 = ORIENTED_EDGE ( 'NONE', *, *, #19877, .T. ) ;
#9269 = AXIS2_PLACEMENT_3D ( 'NONE', #20538, #19164, #3437 ) ;
#9270 = CARTESIAN_POINT ( 'NONE',  ( -15.48395931107686074, 177.8963445608573295, 313.2677653863855767 ) ) ;
#9271 = ORIENTED_EDGE ( 'NONE', *, *, #18630, .T. ) ;
#9272 = ORIENTED_EDGE ( 'NONE', *, *, #18910, .F. ) ;
#9273 = DIRECTION ( 'NONE',  ( -0.9934404589540163366, -0.1135548637187055454, 0.01346653032743023483 ) ) ;
#9274 = VERTEX_POINT ( 'NONE', #3868 ) ;
#9275 = AXIS2_PLACEMENT_3D ( 'NONE', #14244, #2157, #19386 ) ;
#9276 = AXIS2_PLACEMENT_3D ( 'NONE', #8708, #21019, #3666 ) ;
#9277 = CARTESIAN_POINT ( 'NONE',  ( 75.90743353164279483, 96.21294322789843534, 79.81268430165899019 ) ) ;
#9278 = CONTEXT_DEPENDENT_SHAPE_REPRESENTATION ( #923, #227 ) ;
#9279 = VERTEX_POINT ( 'NONE', #21096 ) ;
#9280 = LINE ( 'NONE', #10895, #4853 ) ;
#9281 = EDGE_CURVE ( 'NONE', #21384, #10057, #15100, .T. ) ;
#9282 = EDGE_CURVE ( 'NONE', #6252, #21740, #4268, .T. ) ;
#9283 = FACE_OUTER_BOUND ( 'NONE', #19137, .T. ) ;
#9284 = CONICAL_SURFACE ( 'NONE', #18476, 3.399999999999986144, 1.029744258676653201 ) ;
#9285 = ORIENTED_EDGE ( 'NONE', *, *, #13839, .F. ) ;
#9286 = DIRECTION ( 'NONE',  ( -0.9999164797902015955, -6.965998958219364448E-18, 0.01292414190464157182 ) ) ;
#9287 = EDGE_LOOP ( 'NONE', ( #6814, #19497, #11577, #8942 ) ) ;
#9288 = CARTESIAN_POINT ( 'NONE',  ( 51.38234815825344270, 111.9218655255082524, -48.12259961501336392 ) ) ;
#9289 = ORIENTED_EDGE ( 'NONE', *, *, #6738, .F. ) ;
#9290 = ORIENTED_EDGE ( 'NONE', *, *, #21263, .T. ) ;
#9291 = LINE ( 'NONE', #340, #9243 ) ;
#9292 = CARTESIAN_POINT ( 'NONE',  ( 153.9999999999992610, 1.999999999999998224, 53.76161406891468175 ) ) ;
#9293 = CARTESIAN_POINT ( 'NONE',  ( -62.57984418954151806, 127.0293918815981442, 187.6629419631760243 ) ) ;
#9294 = CARTESIAN_POINT ( 'NONE',  ( -58.31305875343129941, 118.9211851617823328, 168.0010324496986698 ) ) ;
#9295 = VECTOR ( 'NONE', #11104, 999.9999999999998863 ) ;
#9296 = CIRCLE ( 'NONE', #4886, 95.00000000000000000 ) ;
#9297 = VERTEX_POINT ( 'NONE', #16076 ) ;
#9298 = LINE ( 'NONE', #19845, #14533 ) ;
#9299 = CARTESIAN_POINT ( 'NONE',  ( -164.0000000000000000, 1.999999999999998224, 8.000000000000019540 ) ) ;
#9300 = EDGE_LOOP ( 'NONE', ( #8718, #14452, #21930, #14298 ) ) ;
#9301 = VECTOR ( 'NONE', #11962, 1000.000000000000114 ) ;
#9302 = FACE_OUTER_BOUND ( 'NONE', #14214, .T. ) ;
#9303 = CARTESIAN_POINT ( 'NONE',  ( -88.18570483488321088, 88.83504250765321331, 50.51296395271546658 ) ) ;
#9304 = DIRECTION ( 'NONE',  ( -0.001106430228479768352, 0.004756344385284941127, 0.9999880764290332014 ) ) ;
#9305 = VECTOR ( 'NONE', #14541, 1000.000000000000227 ) ;
#9307 = EDGE_LOOP ( 'NONE', ( #10889, #14397, #20747, #4894 ) ) ;
#9306 = VERTEX_POINT ( 'NONE', #2141 ) ;
#9308 = DIRECTION ( 'NONE',  ( 2.449293598294706414E-16, 0.000000000000000000, 1.000000000000000000 ) ) ;
#9309 = CARTESIAN_POINT ( 'NONE',  ( -5.783615788470215513, 81.64368954560637803, -81.51717177438210626 ) ) ;
#9310 = EDGE_LOOP ( 'NONE', ( #17602, #5418, #9628 ) ) ;
#9311 = DIRECTION ( 'NONE',  ( -0.9934404589540163366, -0.1135548637187061005, 0.01346653032743037014 ) ) ;
#9312 = DIRECTION ( 'NONE',  ( 7.125109674161246868E-05, -0.9999848031710252272, 0.005512562950850154186 ) ) ;
#9313 = ORIENTED_EDGE ( 'NONE', *, *, #4824, .F. ) ;
#9314 = PLANE ( 'NONE',  #9758 ) ;
#9315 = LINE ( 'NONE', #16360, #16773 ) ;
#9316 = LINE ( 'NONE', #2317, #17043 ) ;
#9317 = ORIENTED_EDGE ( 'NONE', *, *, #12019, .T. ) ;
#9318 = CARTESIAN_POINT ( 'NONE',  ( 93.06424251235320355, 77.12912189496643123, 28.79962987465162172 ) ) ;
#9319 = VERTEX_POINT ( 'NONE', #21436 ) ;
#9320 = DIRECTION ( 'NONE',  ( 0.000000000000000000, 0.000000000000000000, 1.000000000000000000 ) ) ;
#9321 = CARTESIAN_POINT ( 'NONE',  ( -91.23296681615020987, 78.26422321607698507, -30.58575029229929143 ) ) ;
#9322 = AXIS2_PLACEMENT_3D ( 'NONE', #21702, #5867, #14865 ) ;
#9323 = DIRECTION ( 'NONE',  ( 0.000000000000000000, 0.000000000000000000, 1.000000000000000000 ) ) ;
#9324 = CARTESIAN_POINT ( 'NONE',  ( -41.49342968777003193, 166.0571615038676327, 271.4240548815895977 ) ) ;
#9325 = CARTESIAN_POINT ( 'NONE',  ( 0.000000000000000000, 25.00000000000000000, 0.000000000000000000 ) ) ;
#9326 = ORIENTED_EDGE ( 'NONE', *, *, #10855, .T. ) ;
#9327 = CARTESIAN_POINT ( 'NONE',  ( 58.13288207869166513, 126.2713511641370445, 48.59330799816777358 ) ) ;
#9328 = CYLINDRICAL_SURFACE ( 'NONE', #4197, 2.000000000000001332 ) ;
#9329 = AXIS2_PLACEMENT_3D ( 'NONE', #19691, #5347, #17902 ) ;
#9330 = DIRECTION ( 'NONE',  ( 7.125109674403277385E-05, -0.9999848031710253382, 0.005512562950848281552 ) ) ;
#9331 = EDGE_LOOP ( 'NONE', ( #20581, #3078, #4498, #3558 ) ) ;
#9332 = DIRECTION ( 'NONE',  ( 0.01292394549866733404, 0.005513023399720420534, 0.9999012842304693116 ) ) ;
#9333 = CARTESIAN_POINT ( 'NONE',  ( 0.000000000000000000, 18.00000000000000355, 0.000000000000000000 ) ) ;
#9334 = ORIENTED_EDGE ( 'NONE', *, *, #16777, .F. ) ;
#9335 = ORIENTED_EDGE ( 'NONE', *, *, #8933, .T. ) ;
#9336 = CARTESIAN_POINT ( 'NONE',  ( -105.3709006619169628, 71.09718787230099224, 31.57492962159251348 ) ) ;
#9337 = ORIENTED_EDGE ( 'NONE', *, *, #13936, .T. ) ;
#9338 = CIRCLE ( 'NONE', #22159, 6.250000000000000000 ) ;
#9340 = ORIENTED_EDGE ( 'NONE', *, *, #12902, .T. ) ;
#9339 = VERTEX_POINT ( 'NONE', #315 ) ;
#9341 = CYLINDRICAL_SURFACE ( 'NONE', #8850, 2.000000000000004885 ) ;
#9342 = FACE_OUTER_BOUND ( 'NONE', #18653, .T. ) ;
#9343 = EDGE_CURVE ( 'NONE', #2512, #13022, #5461, .T. ) ;
#9344 = AXIS2_PLACEMENT_3D ( 'NONE', #8468, #2859, #18702 ) ;
#9345 = CARTESIAN_POINT ( 'NONE',  ( -91.86780221137910019, 79.10677575599461875, -26.44518439498801854 ) ) ;
#9346 = CARTESIAN_POINT ( 'NONE',  ( -40.94831321612058161, 169.5761513248267818, 277.1576504944517296 ) ) ;
#9347 = EDGE_CURVE ( 'NONE', #7130, #9297, #15483, .T. ) ;
#9348 = CARTESIAN_POINT ( 'NONE',  ( -38.56531521350737535, 165.8559883853732515, 234.8931899347302874 ) ) ;
#9349 = CARTESIAN_POINT ( 'NONE',  ( 19.68743419676729189, 183.9263611086432775, 315.9693692526456630 ) ) ;
#9350 = CARTESIAN_POINT ( 'NONE',  ( -0.9693106428480923187, 86.14745084375785211, -74.99373598426512899 ) ) ;
#9351 = CARTESIAN_POINT ( 'NONE',  ( 19.43877198876942813, 177.6144908738019694, 111.1987526180507047 ) ) ;
#9352 = ADVANCED_FACE ( 'NONE', ( #1929, #5803, #8916, #3964 ), #205, .T. ) ;
#9353 = DIRECTION ( 'NONE',  ( 0.009760756503428037745, -0.9999378516499562997, 0.005387065077612779827 ) ) ;
#9354 = LINE ( 'NONE', #18436, #5533 ) ;
#9355 = ORIENTED_EDGE ( 'NONE', *, *, #8240, .F. ) ;
#9356 = CARTESIAN_POINT ( 'NONE',  ( -44.25520882077128704, 168.2183454221810734, 273.2074843050344271 ) ) ;
#9357 = ORIENTED_EDGE ( 'NONE', *, *, #8238, .F. ) ;
#9358 = ORIENTED_EDGE ( 'NONE', *, *, #3086, .T. ) ;
#9359 = DIRECTION ( 'NONE',  ( 0.01125613334114312913, 0.4913919529878050807, 0.8708658036695648974 ) ) ;
#9360 = EDGE_CURVE ( 'NONE', #19120, #1243, #89, .T. ) ;
#9361 = B_SPLINE_CURVE_WITH_KNOTS ( 'NONE', 3,
 ( #17983, #7514, #12697, #5662, #5766, #9223 ),
 .UNSPECIFIED., .F., .F.,
 ( 4, 2, 4 ),
 ( 0.009270618776430230440, 0.01189894710419334319, 0.01452727543195645593 ),
 .UNSPECIFIED. ) ;
#9362 = DIRECTION ( 'NONE',  ( 7.125109674161246868E-05, -0.9999848031710252272, 0.005512562950850154186 ) ) ;
#9363 = CARTESIAN_POINT ( 'NONE',  ( 21.90540070143018525, 189.4003865961453528, -109.1087788745517599 ) ) ;
#9364 = CARTESIAN_POINT ( 'NONE',  ( 77.49749086929654140, 75.10304909037273546, 3.426285700830333791 ) ) ;
#9365 = DIRECTION ( 'NONE',  ( -0.9999164797902015955, -8.772500386246549315E-18, 0.01292414190464155101 ) ) ;
#9366 = AXIS2_PLACEMENT_3D ( 'NONE', #6189, #20186, #13442 ) ;
#9367 = CARTESIAN_POINT ( 'NONE',  ( 39.99665919160806027, 170.0000000000000284, -0.5169656761856848970 ) ) ;
#9368 = DIRECTION ( 'NONE',  ( 0.3101392564284310982, 0.9506461370142479383, -0.009250070373107712254 ) ) ;
#9369 = PLANE ( 'NONE',  #123 ) ;
#9370 = ADVANCED_FACE ( 'NONE', ( #12618 ), #10989, .T. ) ;
#9371 = VERTEX_POINT ( 'NONE', #19261 ) ;
#9372 = DIRECTION ( 'NONE',  ( 1.000000000000000000, 0.000000000000000000, 0.000000000000000000 ) ) ;
#9373 = EDGE_LOOP ( 'NONE', ( #6452, #7894, #8754 ) ) ;
#9374 = CARTESIAN_POINT ( 'NONE',  ( 0.000000000000000000, 0.000000000000000000, 0.000000000000000000 ) ) ;
#9375 = CARTESIAN_POINT ( 'NONE',  ( 14.08739029393882802, 113.6767190643319196, 122.7326134183275173 ) ) ;
#9376 = EDGE_CURVE ( 'NONE', #13307, #10113, #8114, .T. ) ;
#9377 = CARTESIAN_POINT ( 'NONE',  ( 90.90077733783162728, 77.56213813822601821, -31.87679858714243153 ) ) ;
#9378 = DIRECTION ( 'NONE',  ( 0.009001891267206851843, -0.4952179990463990711, 0.8687221071056580035 ) ) ;
#9379 = CARTESIAN_POINT ( 'NONE',  ( -90.51848467603900872, 80.22648697776344306, 32.24949179442770486 ) ) ;
#9380 = CARTESIAN_POINT ( 'NONE',  ( 41.56623493000986258, 91.17157287525387233, 82.46967996629570052 ) ) ;
#9381 = ORIENTED_EDGE ( 'NONE', *, *, #1523, .T. ) ;
#9382 = CARTESIAN_POINT ( 'NONE',  ( -15.13015584224213228, 179.6094257463666679, 315.6214976206437655 ) ) ;
#9383 = CARTESIAN_POINT ( 'NONE',  ( -49.61330349940486428, 114.6621811589122757, 166.8870046147178812 ) ) ;
#9384 = CARTESIAN_POINT ( 'NONE',  ( -15.00888604204753385, 180.0069015676392326, 312.9893017111969584 ) ) ;
#9385 = ORIENTED_EDGE ( 'NONE', *, *, #14970, .F. ) ;
#9386 = TOROIDAL_SURFACE ( 'NONE', #22203, 26.23296215977915935, 2.000000000000000000 ) ;
#9387 = ORIENTED_EDGE ( 'NONE', *, *, #22270, .F. ) ;
#9388 = DIRECTION ( 'NONE',  ( 7.176269450075762180E-19, -1.000000000000000000, 5.550596000020001457E-17 ) ) ;
#9389 = ADVANCED_FACE ( 'NONE', ( #17907 ), #16583, .T. ) ;
#9390 = DIRECTION ( 'NONE',  ( 0.01035335185279143318, 0.005513005182356926943, 0.9999312050732649393 ) ) ;
#9391 = DIRECTION ( 'NONE',  ( -1.387778780781445202E-14, 0.000000000000000000, 1.000000000000000000 ) ) ;
#9392 = EDGE_CURVE ( 'NONE', #1720, #16057, #8793, .T. ) ;
#9393 = CARTESIAN_POINT ( 'NONE',  ( 1.117803423002105445, 55.00000000000000000, 109.6947150755565161 ) ) ;
#9394 = ORIENTED_EDGE ( 'NONE', *, *, #3596, .T. ) ;
#9395 = LINE ( 'NONE', #796, #12385 ) ;
#9396 = CARTESIAN_POINT ( 'NONE',  ( -49.85669660544819948, 95.27192509958106825, -43.90954682546798438 ) ) ;
#9397 = EDGE_LOOP ( 'NONE', ( #6345, #4549 ) ) ;
#9398 = CARTESIAN_POINT ( 'NONE',  ( -106.3651776870870833, 78.54983655346497073, -28.04389441634544866 ) ) ;
#9399 = ORIENTED_EDGE ( 'NONE', *, *, #475, .F. ) ;
#9400 = CARTESIAN_POINT ( 'NONE',  ( 13.01890817498768449, 190.3110758050131892, 320.8522954438618058 ) ) ;
#9401 = DIRECTION ( 'NONE',  ( -0.01292394549866731843, -0.005513023399720594006, -0.9999012842304693116 ) ) ;
#9402 = CARTESIAN_POINT ( 'NONE',  ( -2.116856996920899014, 86.19447564219862556, 75.08617727949184939 ) ) ;
#9403 = VERTEX_POINT ( 'NONE', #15455 ) ;
#9404 = FACE_OUTER_BOUND ( 'NONE', #12860, .T. ) ;
#9405 = CARTESIAN_POINT ( 'NONE',  ( -54.52327687265817957, 2.000000000000000000, -111.3697098814011923 ) ) ;
#9406 = EDGE_CURVE ( 'NONE', #3408, #7438, #19475, .T. ) ;
#9407 = EDGE_CURVE ( 'NONE', #17658, #10714, #10155, .T. ) ;
#9408 = ORIENTED_EDGE ( 'NONE', *, *, #7257, .F. ) ;
#9409 = CARTESIAN_POINT ( 'NONE',  ( 41.59445599892145395, 107.1767044522904939, 70.73012046083394466 ) ) ;
#9410 = CARTESIAN_POINT ( 'NONE',  ( -89.37770891450712440, 88.38797322560618852, 50.54303061661246943 ) ) ;
#9411 = APPLICATION_PROTOCOL_DEFINITION ( 'draft international standard', 'automotive_design', 1998, #12488 ) ;
#9412 = VECTOR ( 'NONE', #6447, 1000.000000000000000 ) ;
#9413 = ORIENTED_EDGE ( 'NONE', *, *, #8390, .F. ) ;
#9414 = DIRECTION ( 'NONE',  ( -0.7161863329816251511, -0.003898296230782250828, -0.6978982302147139771 ) ) ;
#9415 = DIRECTION ( 'NONE',  ( -0.9232306267972774094, 0.000000000000000000, 0.3842462878721227826 ) ) ;
#9416 = VERTEX_POINT ( 'NONE', #19814 ) ;
#9417 = CARTESIAN_POINT ( 'NONE',  ( -162.0000000000000000, 20.00000000000000000, -9.999999999999978684 ) ) ;
#9418 = FACE_OUTER_BOUND ( 'NONE', #7705, .T. ) ;
#9419 = CARTESIAN_POINT ( 'NONE',  ( -105.7217631510340681, 70.01235472379876512, -30.37969943364871028 ) ) ;
#9420 = DIRECTION ( 'NONE',  ( 0.01292394549866743812, 0.005513023399720639109, 0.9999012842304693116 ) ) ;
#9421 = CYLINDRICAL_SURFACE ( 'NONE', #4903, 2.000000000000008438 ) ;
#9422 = ORIENTED_EDGE ( 'NONE', *, *, #18226, .F. ) ;
#9423 = CARTESIAN_POINT ( 'NONE',  ( 0.4135725409485815351, 72.00000000000000000, 31.99732735328655053 ) ) ;
#9424 = ORIENTED_EDGE ( 'NONE', *, *, #15604, .T. ) ;
#9425 = CARTESIAN_POINT ( 'NONE',  ( 53.19494802549758106, 127.3639955235004777, 246.8639849220819542 ) ) ;
#9426 = CYLINDRICAL_SURFACE ( 'NONE', #19577, 2.000000000000001332 ) ;
#9427 = DIRECTION ( 'NONE',  ( 0.000000000000000000, 1.000000000000000000, -0.000000000000000000 ) ) ;
#9428 = DIRECTION ( 'NONE',  ( -2.449293598294706414E-16, 0.000000000000000000, -1.000000000000000000 ) ) ;
#9429 = AXIS2_PLACEMENT_3D ( 'NONE', #8975, #8858, #150 ) ;
#9430 = DIRECTION ( 'NONE',  ( 0.9999164797902017066, 0.000000000000000000, -0.01292414190463832269 ) ) ;
#9431 = CARTESIAN_POINT ( 'NONE',  ( -55.33804461215960657, 114.2193244133317904, 167.6379947637574617 ) ) ;
#9432 = CARTESIAN_POINT ( 'NONE',  ( -9.134655005754124701, 81.99999999999998579, -85.72312909216948640 ) ) ;
#9433 = CARTESIAN_POINT ( 'NONE',  ( 39.76222920527046512, 105.5861410271771916, 91.72774381316284575 ) ) ;
#9434 = ORIENTED_EDGE ( 'NONE', *, *, #17945, .T. ) ;
#9435 = FACE_OUTER_BOUND ( 'NONE', #9511, .T. ) ;
#9436 = LINE ( 'NONE', #13251, #8470 ) ;
#9437 = VERTEX_POINT ( 'NONE', #3136 ) ;
#9438 = ORIENTED_EDGE ( 'NONE', *, *, #15379, .F. ) ;
#9439 = CARTESIAN_POINT ( 'NONE',  ( -83.05224505503836951, 75.08638595516889325, 5.128520313100306538 ) ) ;
#9440 = CARTESIAN_POINT ( 'NONE',  ( -90.16487608766178141, 87.18261312935477747, 51.28728107363841104 ) ) ;
#9441 = B_SPLINE_CURVE_WITH_KNOTS ( 'NONE', 3,
 ( #11874, #15444, #10033, #13487, #22397, #15105, #20804, #11754, #1531, #11984 ),
 .UNSPECIFIED., .F., .F.,
 ( 4, 2, 2, 2, 4 ),
 ( 6.509259464525837440E-17, 0.0004376694309007175192, 0.0008753388618013698778, 0.001313008292702022399, 0.001750677723602674703 ),
 .UNSPECIFIED. ) ;
#9443 = ORIENTED_EDGE ( 'NONE', *, *, #7525, .T. ) ;
#9442 = ORIENTED_EDGE ( 'NONE', *, *, #18345, .F. ) ;
#9444 = EDGE_LOOP ( 'NONE', ( #10306, #20992, #4795, #19291 ) ) ;
#9445 = VECTOR ( 'NONE', #17031, 1000.000000000000227 ) ;
#9446 = LINE ( 'NONE', #16816, #15478 ) ;
#9447 = CARTESIAN_POINT ( 'NONE',  ( 40.36543714644568581, 95.16167471844536863, -44.32834889262264255 ) ) ;
#9448 = CARTESIAN_POINT ( 'NONE',  ( -3.208759309630397460, 189.9379666734643592, 274.8508292759004235 ) ) ;
#9449 = CARTESIAN_POINT ( 'NONE',  ( -90.06393689865117835, 72.00000000000000000, 59.85988923254397065 ) ) ;
#9450 = PRODUCT_DEFINITION ( 'UNKNOWN', '', #5499, #10632 ) ;
#9451 = DIRECTION ( 'NONE',  ( 0.000000000000000000, 0.000000000000000000, 1.000000000000000000 ) ) ;
#9452 = ORIENTED_EDGE ( 'NONE', *, *, #2553, .F. ) ;
#9453 = DIRECTION ( 'NONE',  ( 0.9999164797902015955, 6.965998958219364448E-18, -0.01292414190464157182 ) ) ;
#9454 = CARTESIAN_POINT ( 'NONE',  ( 19.93494142535458025, 184.4443040380761829, 278.2191359478135269 ) ) ;
#9455 = CARTESIAN_POINT ( 'NONE',  ( 20.66208571675547745, 181.9457687355336759, 315.3755798616213042 ) ) ;
#9456 = CARTESIAN_POINT ( 'NONE',  ( 93.21002351426731991, 79.82103140525720164, 28.79774562292276840 ) ) ;
#9457 = CIRCLE ( 'NONE', #13156, 6.000000000000000888 ) ;
#9458 = DIRECTION ( 'NONE',  ( 7.125109674160258889E-05, -0.9999848031710252272, 0.005512562950849897447 ) ) ;
#9459 = ADVANCED_FACE ( 'NONE', ( #9489 ), #18647, .F. ) ;
#9460 =( GEOMETRIC_REPRESENTATION_CONTEXT ( 3 ) GLOBAL_UNCERTAINTY_ASSIGNED_CONTEXT ( ( #1881 ) ) GLOBAL_UNIT_ASSIGNED_CONTEXT ( ( #12716, #12261, #3952 ) ) REPRESENTATION_CONTEXT ( 'NONE', 'WORKASPACE' ) );
#9461 = LINE ( 'NONE', #20254, #12144 ) ;
#9462 = CARTESIAN_POINT ( 'NONE',  ( 90.82246629754762068, 169.9999999999999716, -1.173900486973974200 ) ) ;
#9463 = VERTEX_POINT ( 'NONE', #17161 ) ;
#9464 = CARTESIAN_POINT ( 'NONE',  ( 105.4076409534521446, 69.99999999999998579, -33.36508996883003419 ) ) ;
#9465 = ORIENTED_EDGE ( 'NONE', *, *, #19647, .T. ) ;
#9466 = EDGE_CURVE ( 'NONE', #11266, #10714, #13980, .T. ) ;
#9467 = ORIENTED_EDGE ( 'NONE', *, *, #18951, .F. ) ;
#9468 = CARTESIAN_POINT ( 'NONE',  ( -9.804288294571927409, 187.7022783261437837, 321.1616740932373091 ) ) ;
#9469 = CIRCLE ( 'NONE', #3233, 2.000000000000001332 ) ;
#9470 = DIRECTION ( 'NONE',  ( 0.01292414190464131682, 0.000000000000000000, 0.9999164797902017066 ) ) ;
#9471 = CARTESIAN_POINT ( 'NONE',  ( 76.10617011087394701, 75.05943625219154569, -4.352187486329626154 ) ) ;
#9472 = FACE_OUTER_BOUND ( 'NONE', #19832, .T. ) ;
#9473 = CARTESIAN_POINT ( 'NONE',  ( 10.15309714582121714, 176.0218267656414355, 323.4662548820142547 ) ) ;
#9475 = CARTESIAN_POINT ( 'NONE',  ( 1.080781817686064405, 165.4609577950973573, 83.61805050855254251 ) ) ;
#9474 = AXIS2_PLACEMENT_3D ( 'NONE', #3836, #7167, #45 ) ;
#9476 = EDGE_CURVE ( 'NONE', #3676, #9640, #16930, .T. ) ;
#9477 = CARTESIAN_POINT ( 'NONE',  ( 79.99331838321626265, 102.0000000000000000, 3.966068647628679500 ) ) ;
#9478 = EDGE_CURVE ( 'NONE', #6890, #16183, #8462, .T. ) ;
#9479 = ORIENTED_EDGE ( 'NONE', *, *, #19604, .F. ) ;
#9480 = EDGE_CURVE ( 'NONE', #16435, #13022, #5905, .T. ) ;
#9481 = CARTESIAN_POINT ( 'NONE',  ( 65.34146690339817098, 126.1473081376433498, 25.99859803869739139 ) ) ;
#9482 = CARTESIAN_POINT ( 'NONE',  ( -4.048864177140030662, 2.209883817142210827, -313.0895029202206388 ) ) ;
#9483 = CARTESIAN_POINT ( 'NONE',  ( -58.70938816073125111, 114.2401488287702449, 171.4591396250003470 ) ) ;
#9484 = CARTESIAN_POINT ( 'NONE',  ( -40.82592696026183887, 106.8159614793892018, 71.47568422908058494 ) ) ;
#9485 = EDGE_CURVE ( 'NONE', #14385, #21650, #11796, .T. ) ;
#9486 = CARTESIAN_POINT ( 'NONE',  ( 91.92966151681221731, 79.05204536692269812, -28.63995821788549279 ) ) ;
#9487 = CARTESIAN_POINT ( 'NONE',  ( 0.000000000000000000, 0.000000000000000000, 0.000000000000000000 ) ) ;
#9488 = CARTESIAN_POINT ( 'NONE',  ( 1.163172771417732010, 45.00000000000000000, 89.99248318111813205 ) ) ;
#9489 = FACE_OUTER_BOUND ( 'NONE', #19333, .T. ) ;
#9490 = ORIENTED_EDGE ( 'NONE', *, *, #2105, .F. ) ;
#9491 = CIRCLE ( 'NONE', #6178, 10.00000000000000711 ) ;
#9492 = FACE_BOUND ( 'NONE', #22400, .T. ) ;
#9493 = EDGE_LOOP ( 'NONE', ( #19762, #21579, #19698, #11999, #7179, #20560 ) ) ;
#9494 = CARTESIAN_POINT ( 'NONE',  ( 67.43998885458336190, 192.1904093341285886, 33.60813087397579579 ) ) ;
#9495 = CARTESIAN_POINT ( 'NONE',  ( -12.14916032298575921, 182.4209000231529672, 306.6034495403590086 ) ) ;
#9496 = STYLED_ITEM ( 'NONE', ( #12142 ), #2209 ) ;
#9497 = VERTEX_POINT ( 'NONE', #2388 ) ;
#9498 = ADVANCED_FACE ( 'NONE', ( #8410 ), #16414, .T. ) ;
#9499 = VERTEX_POINT ( 'NONE', #21642 ) ;
#9500 = FACE_OUTER_BOUND ( 'NONE', #9300, .T. ) ;
#9501 = ADVANCED_FACE ( 'NONE', ( #18873 ), #11426, .F. ) ;
#9502 = MANIFOLD_SOLID_BREP ( 'Stock-MAS-425-1', #21953 ) ;
#9503 = EDGE_CURVE ( 'NONE', #5306, #5157, #18165, .T. ) ;
#9504 = DIRECTION ( 'NONE',  ( 0.9999164797902017066, 0.000000000000000000, -0.01292414190464117631 ) ) ;
#9505 = CONTEXT_DEPENDENT_SHAPE_REPRESENTATION ( #4850, #3698 ) ;
#9506 = AXIS2_PLACEMENT_3D ( 'NONE', #2652, #7923, #14956 ) ;
#9507 = ADVANCED_FACE ( 'NONE', ( #4849 ), #11993, .F. ) ;
#9508 = DIRECTION ( 'NONE',  ( 0.9934404589540162256, 0.1135548637187056842, -0.01346653032743081423 ) ) ;
#9509 = VECTOR ( 'NONE', #21792, 999.9999999999998863 ) ;
#9510 = FACE_OUTER_BOUND ( 'NONE', #312, .T. ) ;
#9511 = EDGE_LOOP ( 'NONE', ( #20334, #1251, #6171 ) ) ;
#9512 = CARTESIAN_POINT ( 'NONE',  ( 82.94572876491719171, 105.0000000000000000, -72.24960954674284608 ) ) ;
#9513 = ORIENTED_EDGE ( 'NONE', *, *, #20409, .F. ) ;
#9514 = EDGE_CURVE ( 'NONE', #12249, #11335, #1758, .T. ) ;
#9515 = CARTESIAN_POINT ( 'NONE',  ( -12.37189876511640918, 182.1695727904451587, 306.8303737958513580 ) ) ;
#9516 = VERTEX_POINT ( 'NONE', #10595 ) ;
#9517 = CARTESIAN_POINT ( 'NONE',  ( -61.06284936382945716, 114.6696180983937410, 168.3840612900001190 ) ) ;
#9518 = ORIENTED_EDGE ( 'NONE', *, *, #4753, .F. ) ;
#9519 = CARTESIAN_POINT ( 'NONE',  ( 67.23320572660466610, 192.1022009597330680, 17.60971032628828681 ) ) ;
#9520 = CARTESIAN_POINT ( 'NONE',  ( -61.67972807482614428, 191.4143309225244707, 257.3032278304543183 ) ) ;
#9521 = CARTESIAN_POINT ( 'NONE',  ( -18.68000515982659948, 88.26848370977704406, 77.55425219113827495 ) ) ;
#9522 = ORIENTED_EDGE ( 'NONE', *, *, #15583, .T. ) ;
#9523 = CARTESIAN_POINT ( 'NONE',  ( 49.99582398951007889, 170.0000000000000284, -0.6462070952321007367 ) ) ;
#9524 = AXIS2_PLACEMENT_3D ( 'NONE', #19130, #3071, #4893 ) ;
#9525 = CARTESIAN_POINT ( 'NONE',  ( -8.542205542555748821, 185.5086388639571169, 305.9178550086769519 ) ) ;
#9526 = EDGE_CURVE ( 'NONE', #13282, #18526, #6806, .T. ) ;
#9527 = AXIS2_PLACEMENT_3D ( 'NONE', #1706, #10653, #6972 ) ;
#9528 = ORIENTED_EDGE ( 'NONE', *, *, #6148, .T. ) ;
#9529 = UNCERTAINTY_MEASURE_WITH_UNIT (LENGTH_MEASURE( 1.000000000000000082E-05 ), #3784, 'distance_accuracy_value', 'NONE');
#9530 = DIRECTION ( 'NONE',  ( -0.01292394549866632963, -0.005513023399716958026, -0.9999012842304692006 ) ) ;
#9531 = CARTESIAN_POINT ( 'NONE',  ( -89.46067271499279627, 89.11592295107170969, 51.60461869884851183 ) ) ;
#9532 = APPLICATION_PROTOCOL_DEFINITION ( 'draft international standard', 'automotive_design', 1998, #14106 ) ;
#9533 = ORIENTED_EDGE ( 'NONE', *, *, #16659, .T. ) ;
#9534 = CARTESIAN_POINT ( 'NONE',  ( 3.603563735215878250, 37.00000000000000711, -86.34855356100663926 ) ) ;
#9535 = CARTESIAN_POINT ( 'NONE',  ( -51.53950506418888722, 113.3113159538933559, -43.52567687456358669 ) ) ;
#9536 = ORIENTED_EDGE ( 'NONE', *, *, #15974, .F. ) ;
#9537 = LINE ( 'NONE', #20086, #19854 ) ;
#9538 = CARTESIAN_POINT ( 'NONE',  ( 3.982207582136937596, 166.6986315483347028, 308.0958888182936448 ) ) ;
#9539 = ORIENTED_EDGE ( 'NONE', *, *, #16690, .F. ) ;
#9540 = VECTOR ( 'NONE', #19480, 1000.000000000000227 ) ;
#9541 = MANIFOLD_SOLID_BREP ( 'Stock-MAS-425-1', #2172 ) ;
#9542 = CARTESIAN_POINT ( 'NONE',  ( 51.50086788761742440, 181.5071008296286266, 255.8949677505804061 ) ) ;
#9543 = PRODUCT ( 'MAS-425', 'MAS-425', '', ( #2180 ) ) ;
#9544 = VECTOR ( 'NONE', #8044, 1000.000000000000114 ) ;
#9545 = CARTESIAN_POINT ( 'NONE',  ( 153.9999999999992610, 1.999999999999998224, -53.76161406891471017 ) ) ;
#9546 = ORIENTED_EDGE ( 'NONE', *, *, #18894, .F. ) ;
#9547 = ADVANCED_FACE ( 'NONE', ( #5187 ), #17399, .F. ) ;
#9548 = DIRECTION ( 'NONE',  ( -0.9250486434174662875, -0.3795887553195633202, 0.01404934683357507604 ) ) ;
#9549 = ORIENTED_EDGE ( 'NONE', *, *, #6112, .T. ) ;
#9550 = DIRECTION ( 'NONE',  ( -0.5089394657577703818, -0.004781488884709769391, -0.8607890319690654213 ) ) ;
#9551 = CARTESIAN_POINT ( 'NONE',  ( -93.06424251235314671, 77.12912189496638860, -28.79962987465164304 ) ) ;
#9552 = PRODUCT_DEFINITION_FORMATION_WITH_SPECIFIED_SOURCE ( 'ANY', '', #9749, .NOT_KNOWN. ) ;
#9553 = CARTESIAN_POINT ( 'NONE',  ( -55.33837949231430287, 118.9192529882356268, 167.6120857178884762 ) ) ;
#9554 = CARTESIAN_POINT ( 'NONE',  ( -38.76986306108200608, 107.0090700318704933, 91.89681970336006600 ) ) ;
#9555 = ORIENTED_EDGE ( 'NONE', *, *, #11609, .T. ) ;
#9556 = CARTESIAN_POINT ( 'NONE',  ( -9.472248412593200939, 69.99999999999998579, -86.53426659026914081 ) ) ;
#9557 = DIRECTION ( 'NONE',  ( -0.009985269297354625040, -0.6348858185549794975, -0.7725414498878574454 ) ) ;
#9558 = AXIS2_PLACEMENT_3D ( 'NONE', #17452, #13879, #1590 ) ;
#9559 = CARTESIAN_POINT ( 'NONE',  ( 41.02615909384066839, 106.6902466465767105, 92.47289523622401930 ) ) ;
#9560 = VERTEX_POINT ( 'NONE', #8735 ) ;
#9561 = LINE ( 'NONE', #16596, #15727 ) ;
#9562 = EDGE_CURVE ( 'NONE', #367, #16244, #8967, .T. ) ;
#9563 = ORIENTED_EDGE ( 'NONE', *, *, #5379, .T. ) ;
#9564 = VERTEX_POINT ( 'NONE', #3237 ) ;
#9565 = AXIS2_PLACEMENT_3D ( 'NONE', #8325, #1240, #22640 ) ;
#9566 = CARTESIAN_POINT ( 'NONE',  ( -83.31183079427971450, 75.07749829403635999, 4.920832620970953641 ) ) ;
#9567 = CIRCLE ( 'NONE', #2597, 3.309500000000002107 ) ;
#9568 = CARTESIAN_POINT ( 'NONE',  ( -88.16163815486164879, 88.05173128619230738, 53.06165861546533336 ) ) ;
#9569 = VECTOR ( 'NONE', #2929, 1000.000000000000000 ) ;
#9570 = ORIENTED_EDGE ( 'NONE', *, *, #14157, .F. ) ;
#9571 = DIRECTION ( 'NONE',  ( 0.1136178953597579422, -0.9935164314186355483, 0.004009283626633659663 ) ) ;
#9572 = ORIENTED_EDGE ( 'NONE', *, *, #17774, .F. ) ;
#9573 = VERTEX_POINT ( 'NONE', #18981 ) ;
#9574 = VECTOR ( 'NONE', #5095, 999.9999999999998863 ) ;
#9575 = CARTESIAN_POINT ( 'NONE',  ( -58.84901841222320229, 118.8937358571614453, 163.0286266904498405 ) ) ;
#9576 = CARTESIAN_POINT ( 'NONE',  ( 58.10057221494500368, 126.2575686056377435, 46.09355478759161429 ) ) ;
#9577 = CARTESIAN_POINT ( 'NONE',  ( -41.58451242677340076, 92.58578643762699301, -83.88377541325534992 ) ) ;
#9578 = CARTESIAN_POINT ( 'NONE',  ( -37.92407594442742180, 93.21315326087319875, 85.17437120064224132 ) ) ;
#9579 = EDGE_CURVE ( 'NONE', #13714, #22032, #3104, .T. ) ;
#9580 = ORIENTED_EDGE ( 'NONE', *, *, #8215, .T. ) ;
#9581 = EDGE_CURVE ( 'NONE', #6852, #5956, #15258, .T. ) ;
#9582 = DIRECTION ( 'NONE',  ( 0.000000000000000000, 1.000000000000000000, -0.000000000000000000 ) ) ;
#9583 = CARTESIAN_POINT ( 'NONE',  ( 13.80637996605699769, 137.5572120012638777, 100.9913744321402902 ) ) ;
#9584 = CARTESIAN_POINT ( 'NONE',  ( 19.41373208432103681, 183.2702314132801007, 319.1152548829093689 ) ) ;
#9585 = CARTESIAN_POINT ( 'NONE',  ( 44.03028354117878251, 168.0879242961143518, -75.31593853751020617 ) ) ;
#9586 = AXIS2_PLACEMENT_3D ( 'NONE', #18114, #20255, #4518 ) ;
#9587 = DIRECTION ( 'NONE',  ( 0.8981428216242033358, 0.000000000000000000, -0.4397038457472424167 ) ) ;
#9588 = ORIENTED_EDGE ( 'NONE', *, *, #18628, .F. ) ;
#9589 = VECTOR ( 'NONE', #6098, 1000.000000000000000 ) ;
#9590 = SHAPE_REPRESENTATION ( 'Lead Screw Drive Shaft', ( #6292 ), #9963 ) ;
#9591 = AXIS2_PLACEMENT_3D ( 'NONE', #9585, #16619, #2698 ) ;
#9592 = VECTOR ( 'NONE', #8206, 999.9999999999998863 ) ;
#9593 = CARTESIAN_POINT ( 'NONE',  ( 0.000000000000000000, 0.000000000000000000, 0.000000000000000000 ) ) ;
#9594 = ORIENTED_EDGE ( 'NONE', *, *, #3870, .T. ) ;
#9595 = CARTESIAN_POINT ( 'NONE',  ( -90.17340641399441381, 87.01242838177741135, 51.39043932755232902 ) ) ;
#9596 = ORIENTED_EDGE ( 'NONE', *, *, #14367, .F. ) ;
#9597 = PRODUCT_RELATED_PRODUCT_CATEGORY ( 'part', '', ( #18346 ) ) ;
#9598 = DIRECTION ( 'NONE',  ( 5.440186201345738641E-18, 1.000000000000000000, 1.334940939666364181E-17 ) ) ;
#9599 = VERTEX_POINT ( 'NONE', #8865 ) ;
#9600 = VECTOR ( 'NONE', #8529, 1000.000000000000000 ) ;
#9601 =( GEOMETRIC_REPRESENTATION_CONTEXT ( 3 ) GLOBAL_UNCERTAINTY_ASSIGNED_CONTEXT ( ( #14075 ) ) GLOBAL_UNIT_ASSIGNED_CONTEXT ( ( #5329, #523, #20022 ) ) REPRESENTATION_CONTEXT ( 'NONE', 'WORKASPACE' ) );
#9602 = CYLINDRICAL_SURFACE ( 'NONE', #6172, 2.000000000000001332 ) ;
#9603 = LINE ( 'NONE', #2477, #9239 ) ;
#9604 = VECTOR ( 'NONE', #14969, 1000.000000000000114 ) ;
#9605 = CARTESIAN_POINT ( 'NONE',  ( 163.1715728752537018, -1.082576183735519500E-15, -8.828427124748447596 ) ) ;
#9606 = DIRECTION ( 'NONE',  ( 0.9934404589540162256, 0.1135548637187059617, -0.01346653032742970747 ) ) ;
#9607 = EDGE_CURVE ( 'NONE', #17671, #10325, #6916, .T. ) ;
#9608 = CARTESIAN_POINT ( 'NONE',  ( -34.77131261570284693, 119.7725967263615985, 250.0430214605738968 ) ) ;
#9609 = CIRCLE ( 'NONE', #14399, 5.100000000000004974 ) ;
#9610 = VERTEX_POINT ( 'NONE', #12227 ) ;
#9611 = CARTESIAN_POINT ( 'NONE',  ( 8.732865712828660421, 190.3249964942741883, 274.4707185275763095 ) ) ;
#9612 = VERTEX_POINT ( 'NONE', #10494 ) ;
#9613 = CARTESIAN_POINT ( 'NONE',  ( 0.000000000000000000, 0.000000000000000000, 0.000000000000000000 ) ) ;
#9614 = DIRECTION ( 'NONE',  ( 2.025474946048326158E-22, -1.000000000000000000, 1.876735158486679638E-22 ) ) ;
#9615 = CARTESIAN_POINT ( 'NONE',  ( 4.045115290395937535, 144.9647869746168283, 296.7137714017214876 ) ) ;
#9616 = CARTESIAN_POINT ( 'NONE',  ( 68.71681667565954399, 72.00000000000000000, -85.89527988174788220 ) ) ;
#9617 = CARTESIAN_POINT ( 'NONE',  ( -8.663799671886042830, 185.9178481321715424, 321.2345653191283645 ) ) ;
#9618 = CARTESIAN_POINT ( 'NONE',  ( 92.60113547278147905, 70.26667278203287026, 59.37223626620095729 ) ) ;
#9619 = ORIENTED_EDGE ( 'NONE', *, *, #3728, .F. ) ;
#9620 = AXIS2_PLACEMENT_3D ( 'NONE', #11623, #22370, #1398 ) ;
#9621 = CARTESIAN_POINT ( 'NONE',  ( -41.94137166082473556, 162.5796238295972671, 273.2086669205137355 ) ) ;
#9622 = CIRCLE ( 'NONE', #22421, 7.500000000000002665 ) ;
#9623 = DIRECTION ( 'NONE',  ( 0.01292414190464131682, 1.902755938799531179E-22, 0.9999164797902017066 ) ) ;
#9624 = CARTESIAN_POINT ( 'NONE',  ( -14.77708621466310035, 180.6116793951536579, 312.1350740694625756 ) ) ;
#9625 = VERTEX_POINT ( 'NONE', #10717 ) ;
#9626 = CIRCLE ( 'NONE', #12868, 1.999999999999973799 ) ;
#9627 = VERTEX_POINT ( 'NONE', #15566 ) ;
#9628 = ORIENTED_EDGE ( 'NONE', *, *, #12205, .T. ) ;
#9629 = CARTESIAN_POINT ( 'NONE',  ( -64.03197570747913403, 99.62212517233105302, 75.31426563926737572 ) ) ;
#9630 = EDGE_CURVE ( 'NONE', #1331, #16920, #15601, .T. ) ;
#9631 = VECTOR ( 'NONE', #13708, 1000.000000000000000 ) ;
#9632 = MANIFOLD_SOLID_BREP ( 'Stock-MAS-425-1', #10036 ) ;
#9633 = CARTESIAN_POINT ( 'NONE',  ( 12.68111155422823266, 190.1386086654728160, 307.8189900089453772 ) ) ;
#9634 = CONICAL_SURFACE ( 'NONE', #22437, 2.499999999999988010, 1.029744258676651425 ) ;
#9635 = CIRCLE ( 'NONE', #448, 109.9999999999999716 ) ;
#9636 = VECTOR ( 'NONE', #4502, 999.9999999999998863 ) ;
#9637 = CARTESIAN_POINT ( 'NONE',  ( 20.70083805927512088, 149.3646325075532957, 278.4026507072620120 ) ) ;
#9638 = DIRECTION ( 'NONE',  ( 0.9999164797902015955, 6.965998958219364448E-18, -0.01292414190464157182 ) ) ;
#9639 = ADVANCED_FACE ( 'NONE', ( #2201 ), #157, .F. ) ;
#9640 = VERTEX_POINT ( 'NONE', #5528 ) ;
#9641 = CARTESIAN_POINT ( 'NONE',  ( 157.5176307659770885, 0.000000000000000000, -60.94675664190840081 ) ) ;
#9642 = EDGE_CURVE ( 'NONE', #17220, #99, #2552, .T. ) ;
#9643 = CARTESIAN_POINT ( 'NONE',  ( -9.397814517978851256, 184.8013626690785429, 305.2958327382877997 ) ) ;
#9644 = EDGE_LOOP ( 'NONE', ( #11105, #13418 ) ) ;
#9645 = FACE_OUTER_BOUND ( 'NONE', #19143, .T. ) ;
#9646 = CARTESIAN_POINT ( 'NONE',  ( -41.39699765238108853, 125.7553391191873544, -43.72538199251495428 ) ) ;
#9647 = ORIENTED_EDGE ( 'NONE', *, *, #11041, .F. ) ;
#9648 = ORIENTED_EDGE ( 'NONE', *, *, #11390, .T. ) ;
#9649 = DIRECTION ( 'NONE',  ( 0.8637520339192008567, 0.002839416958727990648, 0.5039090806998601790 ) ) ;
#9650 = AXIS2_PLACEMENT_3D ( 'NONE', #21548, #5711, #568 ) ;
#9651 = AXIS2_PLACEMENT_3D ( 'NONE', #14870, #3920, #21924 ) ;
#9652 = DIRECTION ( 'NONE',  ( -2.025474946048326158E-22, 1.000000000000000000, -1.876735158486679638E-22 ) ) ;
#9653 = EDGE_CURVE ( 'NONE', #10899, #13090, #609, .T. ) ;
#9654 = ORIENTED_EDGE ( 'NONE', *, *, #18538, .T. ) ;
#9655 = DIRECTION ( 'NONE',  ( 7.125109674160258889E-05, -0.9999848031710252272, 0.005512562950849897447 ) ) ;
#9656 = CARTESIAN_POINT ( 'NONE',  ( -89.84471876097053666, 87.96141862524974897, 50.80991467805918660 ) ) ;
#9657 = EDGE_CURVE ( 'NONE', #7993, #10504, #21447, .T. ) ;
#9658 = B_SPLINE_CURVE_WITH_KNOTS ( 'NONE', 3,
 ( #19505, #21470, #15628, #21518 ),
 .UNSPECIFIED., .F., .F.,
 ( 4, 4 ),
 ( 0.000000000000000000, 0.001461243987307977218 ),
 .UNSPECIFIED. ) ;
#9659 = APPLICATION_PROTOCOL_DEFINITION ( 'draft international standard', 'automotive_design', 1998, #11311 ) ;
#9661 = EDGE_LOOP ( 'NONE', ( #9185, #11093 ) ) ;
#9660 = VERTEX_POINT ( 'NONE', #13033 ) ;
#9662 = DIRECTION ( 'NONE',  ( 0.4397038457472313144, 0.000000000000000000, -0.8981428216242086648 ) ) ;
#9663 = CARTESIAN_POINT ( 'NONE',  ( -50.94859746947806656, 110.3466764521169807, -46.22168700684313336 ) ) ;
#9664 = CARTESIAN_POINT ( 'NONE',  ( 13.08556214908078985, 190.2789432977352533, 320.8465702879597643 ) ) ;
#9665 = DIRECTION ( 'NONE',  ( 7.125109674161246868E-05, -0.9999848031710252272, 0.005512562950850154186 ) ) ;
#9666 = CARTESIAN_POINT ( 'NONE',  ( -42.64894290516974706, 118.1474297122749135, 27.43850586800562752 ) ) ;
#9667 = AXIS2_PLACEMENT_3D ( 'NONE', #6413, #9848, #18912 ) ;
#9668 = CARTESIAN_POINT ( 'NONE',  ( -7.475646132950418021, 81.19615242270661781, -81.73701953211944726 ) ) ;
#9669 = ORIENTED_EDGE ( 'NONE', *, *, #19556, .T. ) ;
#9670 = EDGE_CURVE ( 'NONE', #4261, #17346, #6774, .T. ) ;
#9671 = CARTESIAN_POINT ( 'NONE',  ( 64.42223680557074772, 144.7550503794368524, -45.19787522242825162 ) ) ;
#9672 = EDGE_LOOP ( 'NONE', ( #16771, #4065, #9518, #3285 ) ) ;
#9673 = CARTESIAN_POINT ( 'NONE',  ( 41.44900574491364154, 144.7660764262362818, -42.90080446601865560 ) ) ;
#9674 = DIRECTION ( 'NONE',  ( 1.000000000000000000, -0.000000000000000000, 1.362186893977296347E-14 ) ) ;
#9675 = CARTESIAN_POINT ( 'NONE',  ( -42.64894290516974706, 118.1474297122749135, 27.43850586800562752 ) ) ;
#9676 = DIRECTION ( 'NONE',  ( -0.01292394549866741384, -0.005513023399720269613, -0.9999012842304692006 ) ) ;
#9677 = ORIENTED_EDGE ( 'NONE', *, *, #3759, .T. ) ;
#9678 = LINE ( 'NONE', #16370, #14808 ) ;
#9679 = SURFACE_SIDE_STYLE ('',( #22164 ) ) ;
#9680 = CARTESIAN_POINT ( 'NONE',  ( 88.82263333796723259, 169.9999999999999716, -1.148052203164690033 ) ) ;
#9681 = CLOSED_SHELL ( 'NONE', ( #22548, #9501, #8559, #17231, #18577, #1797, #14213, #10501, #21083, #15961, #13553, #9788, #4993, #7010, #4035, #14998, #10477, #1665, #20031, #18726, #14338, #1674, #9235, #12341, #787, #16527, #1844, #4505 ) ) ;
#9682 = AXIS2_PLACEMENT_3D ( 'NONE', #3047, #10069, #8109 ) ;
#9683 = ORIENTED_EDGE ( 'NONE', *, *, #15039, .F. ) ;
#9684 = FACE_OUTER_BOUND ( 'NONE', #11134, .T. ) ;
#9685 = ORIENTED_EDGE ( 'NONE', *, *, #106, .T. ) ;
#9686 = AXIS2_PLACEMENT_3D ( 'NONE', #20114, #13050, #21942 ) ;
#9687 = ORIENTED_EDGE ( 'NONE', *, *, #1053, .T. ) ;
#9688 = AXIS2_PLACEMENT_3D ( 'NONE', #3935, #5892, #16272 ) ;
#9689 = DIRECTION ( 'NONE',  ( 0.7912924530843117310, -0.6113994113550570431, -0.006856638134102506846 ) ) ;
#9690 = CARTESIAN_POINT ( 'NONE',  ( -90.17158066196779487, 87.09867769988316866, 51.33820610053523126 ) ) ;
#9691 = EDGE_CURVE ( 'NONE', #1325, #12915, #11564, .T. ) ;
#9692 = CARTESIAN_POINT ( 'NONE',  ( 17.14183078491316436, 175.4877217292663545, 88.23789649046089778 ) ) ;
#9693 = LINE ( 'NONE', #16603, #17402 ) ;
#9694 = ORIENTED_EDGE ( 'NONE', *, *, #17363, .T. ) ;
#9695 = CYLINDRICAL_SURFACE ( 'NONE', #11462, 10.00000000000001599 ) ;
#9696 = LINE ( 'NONE', #16720, #15741 ) ;
#9697 = VECTOR ( 'NONE', #21254, 999.9999999999998863 ) ;
#9698 = CARTESIAN_POINT ( 'NONE',  ( -89.78684647853550871, 79.34753190266584966, 29.57356476272790502 ) ) ;
#9699 = LINE ( 'NONE', #13263, #6915 ) ;
#9700 = CARTESIAN_POINT ( 'NONE',  ( -38.11897055289185232, 96.20077349746044604, 84.87487045055679857 ) ) ;
#9701 = EDGE_CURVE ( 'NONE', #9820, #18018, #9083, .T. ) ;
#9702 = ORIENTED_EDGE ( 'NONE', *, *, #10996, .F. ) ;
#9703 = ORIENTED_EDGE ( 'NONE', *, *, #2357, .T. ) ;
#9704 = CARTESIAN_POINT ( 'NONE',  ( -54.77086557510170906, 114.8307698053962156, 171.9727639297506414 ) ) ;
#9705 = CARTESIAN_POINT ( 'NONE',  ( 74.26458564358016190, 75.03487962395588795, -3.541144389642402857 ) ) ;
#9706 = CARTESIAN_POINT ( 'NONE',  ( 19.05256028926003964, 183.6015641263033444, 317.6936443219116768 ) ) ;
#9707 = VECTOR ( 'NONE', #1583, 999.9999999999998863 ) ;
#9708 = FACE_OUTER_BOUND ( 'NONE', #11187, .T. ) ;
#9709 = AXIS2_PLACEMENT_3D ( 'NONE', #6961, #14467, #13985 ) ;
#9710 = DIRECTION ( 'NONE',  ( -0.4397038457472309814, 0.000000000000000000, -0.8981428216242088869 ) ) ;
#9711 =( REPRESENTATION_RELATIONSHIP ('NONE','NONE', #11808, #14914 ) REPRESENTATION_RELATIONSHIP_WITH_TRANSFORMATION ( #11494 )SHAPE_REPRESENTATION_RELATIONSHIP( ) );
#9712 = FACE_OUTER_BOUND ( 'NONE', #10651, .T. ) ;
#9713 = DIRECTION ( 'NONE',  ( 0.9999164797902015955, 6.965998958219364448E-18, -0.01292414190464157182 ) ) ;
#9714 = ORIENTED_EDGE ( 'NONE', *, *, #9226, .F. ) ;
#9715 = CIRCLE ( 'NONE', #1275, 3.399999999999991918 ) ;
#9716 = CARTESIAN_POINT ( 'NONE',  ( 65.44450461302918143, 145.1911235850906223, 33.89305669233311136 ) ) ;
#9717 = ORIENTED_EDGE ( 'NONE', *, *, #10409, .F. ) ;
#9718 = VERTEX_POINT ( 'NONE', #21262 ) ;
#9719 = DIRECTION ( 'NONE',  ( -2.025474946048326158E-22, 1.000000000000000000, -1.876735158486679638E-22 ) ) ;
#9720 = EDGE_CURVE ( 'NONE', #4427, #20375, #7524, .T. ) ;
#9721 = ORIENTED_EDGE ( 'NONE', *, *, #17572, .T. ) ;
#9722 = EDGE_CURVE ( 'NONE', #11619, #20328, #7681, .T. ) ;
#9723 = AXIS2_PLACEMENT_3D ( 'NONE', #1237, #11793, #3049 ) ;
#9724 = AXIS2_PLACEMENT_3D ( 'NONE', #17458, #13777, #3298 ) ;
#9725 = ORIENTED_EDGE ( 'NONE', *, *, #20428, .T. ) ;
#9726 = CARTESIAN_POINT ( 'NONE',  ( 79.39526044036306018, 75.13524200571961842, 4.041958712526196429 ) ) ;
#9727 = FACE_OUTER_BOUND ( 'NONE', #236, .T. ) ;
#9728 = CARTESIAN_POINT ( 'NONE',  ( 49.40009966013455056, 96.21415597129798414, -46.73627471826173974 ) ) ;
#9729 = DIRECTION ( 'NONE',  ( -0.01292394549866741557, -0.005513023399720270480, -0.9999012842304693116 ) ) ;
#9730 =( BOUNDED_CURVE ( )  B_SPLINE_CURVE ( 3, ( #19147, #8582, #6856, #8350 ),
 .UNSPECIFIED., .F., .T. ) 
 B_SPLINE_CURVE_WITH_KNOTS ( ( 4, 4 ),
 ( 1.570796326794896558, 3.141592653589793116 ),
 .UNSPECIFIED. ) 
 CURVE ( )  GEOMETRIC_REPRESENTATION_ITEM ( )  RATIONAL_B_SPLINE_CURVE ( ( 1.000000000000000000, 0.8047378541243649375, 0.8047378541243649375, 1.000000000000000000 ) ) 
 REPRESENTATION_ITEM ( '' )  );
#9731 = ORIENTED_EDGE ( 'NONE', *, *, #14599, .T. ) ;
#9732 = CARTESIAN_POINT ( 'NONE',  ( -68.99891043397279589, 92.11203426037263853, 85.66888312730651478 ) ) ;
#9733 = DIRECTION ( 'NONE',  ( 1.000000000000000000, 0.000000000000000000, 0.000000000000000000 ) ) ;
#9734 = AXIS2_PLACEMENT_3D ( 'NONE', #15790, #7039, #15913 ) ;
#9735 = CARTESIAN_POINT ( 'NONE',  ( -67.12230846849016075, 89.94961994313915454, 67.62393891741413654 ) ) ;
#9736 = CARTESIAN_POINT ( 'NONE',  ( -41.08973838174756565, 106.8061942917681790, 71.47038841247318430 ) ) ;
#9737 = DIRECTION ( 'NONE',  ( -0.4397038457472424167, 0.000000000000000000, 0.8981428216242032248 ) ) ;
#9738 = CARTESIAN_POINT ( 'NONE',  ( -8.424310978314924370, 185.3118195958672345, 323.2514892018872956 ) ) ;
#9739 = CARTESIAN_POINT ( 'NONE',  ( 23.22251776072470619, 138.3748544051812246, 249.1908735552227938 ) ) ;
#9740 = VERTEX_POINT ( 'NONE', #12684 ) ;
#9741 = CARTESIAN_POINT ( 'NONE',  ( -1.163172771417702700, 81.99999999999998579, -89.99248318111824574 ) ) ;
#9742 = ORIENTED_EDGE ( 'NONE', *, *, #20790, .T. ) ;
#9743 = LINE ( 'NONE', #9494, #20554 ) ;
#9744 = CARTESIAN_POINT ( 'NONE',  ( -13.52657357758894996, 183.2391904061878165, 309.9735533623801871 ) ) ;
#9745 = ORIENTED_EDGE ( 'NONE', *, *, #11185, .T. ) ;
#9746 = ORIENTED_EDGE ( 'NONE', *, *, #16777, .T. ) ;
#9747 = EDGE_CURVE ( 'NONE', #22315, #13904, #7717, .T. ) ;
#9748 = VECTOR ( 'NONE', #14155, 1000.000000000000227 ) ;
#9749 = PRODUCT ( 'Socket Head Cap Screw L', 'Socket Head Cap Screw L', '', ( #18498 ) ) ;
#9750 = CARTESIAN_POINT ( 'NONE',  ( -164.0000000000000000, 20.00000000000000000, -7.999999999999979572 ) ) ;
#9751 = DIRECTION ( 'NONE',  ( 0.01292394549866743812, 0.005513023399720639109, 0.9999012842304693116 ) ) ;
#9752 = DIRECTION ( 'NONE',  ( 0.01292394549866740169, 0.005513023399720822990, 0.9999012842304693116 ) ) ;
#9753 = ORIENTED_EDGE ( 'NONE', *, *, #15175, .F. ) ;
#9754 = CARTESIAN_POINT ( 'NONE',  ( 11.80916335469752987, 187.7920945708437728, 307.7671702419516464 ) ) ;
#9755 = DIRECTION ( 'NONE',  ( 0.9999164797902015955, 6.965998958219364448E-18, -0.01292414190464157182 ) ) ;
#9756 = CARTESIAN_POINT ( 'NONE',  ( -146.5000000000000000, 18.00000000000000355, 2.081668171172168513E-14 ) ) ;
#9757 = CARTESIAN_POINT ( 'NONE',  ( -38.90493699201700650, 97.20305277476600736, 83.98778727448713255 ) ) ;
#9758 = AXIS2_PLACEMENT_3D ( 'NONE', #9542, #21696, #14622 ) ;
#9759 = DIRECTION ( 'NONE',  ( 0.01292394549866745720, 0.005513023399720816918, 0.9999012842304693116 ) ) ;
#9760 = VERTEX_POINT ( 'NONE', #9203 ) ;
#9761 = CARTESIAN_POINT ( 'NONE',  ( -11.46885069223597853, 81.99999999999998579, -91.33151364841880593 ) ) ;
#9762 = CARTESIAN_POINT ( 'NONE',  ( 67.23655452815148692, 145.1029152106949027, 17.86880078497820179 ) ) ;
#9763 = ORIENTED_EDGE ( 'NONE', *, *, #11452, .T. ) ;
#9764 = UNCERTAINTY_MEASURE_WITH_UNIT (LENGTH_MEASURE( 1.000000000000000082E-05 ), #15931, 'distance_accuracy_value', 'NONE');
#9765 = ADVANCED_FACE ( 'NONE', ( #10941 ), #9328, .T. ) ;
#9766 = CARTESIAN_POINT ( 'NONE',  ( 4.182528737366220106, 166.7840834110302808, 323.5943587238651276 ) ) ;
#9767 = DIRECTION ( 'NONE',  ( 2.025474946048326158E-22, -1.000000000000000000, 1.876735158486679638E-22 ) ) ;
#9768 = SHAPE_DEFINITION_REPRESENTATION ( #6248, #3137 ) ;
#9770 = EDGE_LOOP ( 'NONE', ( #7568, #7297, #21008, #3518 ) ) ;
#9769 = EDGE_LOOP ( 'NONE', ( #17282, #1080, #21971, #15618, #22338 ) ) ;
#9771 = FACE_OUTER_BOUND ( 'NONE', #10268, .T. ) ;
#9772 = CARTESIAN_POINT ( 'NONE',  ( -51.34796203869380093, 109.5896734486573791, -43.50763308276343366 ) ) ;
#9773 = CARTESIAN_POINT ( 'NONE',  ( 13.31679592837081572, 190.1462100374990030, 320.8234512119713031 ) ) ;
#9774 = CARTESIAN_POINT ( 'NONE',  ( 63.56236266363622889, 189.3893605493459233, -111.6473409898501075 ) ) ;
#9775 = DIRECTION ( 'NONE',  ( -7.125109674364536131E-05, 0.9999848031710253382, -0.005512562950849706628 ) ) ;
#9776 = DIRECTION ( 'NONE',  ( 0.01292394549866739996, 0.005513023399720822122, 0.9999012842304692006 ) ) ;
#9777 = CARTESIAN_POINT ( 'NONE',  ( 65.90110554552377664, 105.0000000000000000, 69.29678410920483600 ) ) ;
#9778 = DIRECTION ( 'NONE',  ( -0.02033837109167977927, -0.03960957306447945164, -0.9990082243820552765 ) ) ;
#9779 = EDGE_CURVE ( 'NONE', #3163, #11891, #12312, .T. ) ;
#9780 = ORIENTED_EDGE ( 'NONE', *, *, #17432, .F. ) ;
#9781 = LINE ( 'NONE', #9883, #1835 ) ;
#9782 = CARTESIAN_POINT ( 'NONE',  ( 0.000000000000000000, 0.000000000000000000, 0.000000000000000000 ) ) ;
#9783 = ORIENTED_EDGE ( 'NONE', *, *, #11663, .T. ) ;
#9784 = FACE_OUTER_BOUND ( 'NONE', #3670, .T. ) ;
#9785 = CARTESIAN_POINT ( 'NONE',  ( -80.22026031257210832, 86.08487693883552083, 75.35739733108806604 ) ) ;
#9786 = CARTESIAN_POINT ( 'NONE',  ( -1.632550740186649252, 142.7036636415817838, 274.8672572718561469 ) ) ;
#9787 = CARTESIAN_POINT ( 'NONE',  ( -41.41899454747532161, 166.0889136240114681, 277.1829612759436827 ) ) ;
#9788 = ADVANCED_FACE ( 'NONE', ( #4029, #19880 ), #11058, .T. ) ;
#9789 = LINE ( 'NONE', #1402, #15921 ) ;
#9790 = ORIENTED_EDGE ( 'NONE', *, *, #666, .T. ) ;
#9791 = CARTESIAN_POINT ( 'NONE',  ( 47.99676178238597402, 166.7168410604182327, 231.7264817597146020 ) ) ;
#9792 = CARTESIAN_POINT ( 'NONE',  ( 65.83936723693913962, 101.1708071963161615, 64.52020763367299594 ) ) ;
#9793 = ORIENTED_EDGE ( 'NONE', *, *, #20455, .T. ) ;
#9794 = EDGE_CURVE ( 'NONE', #3243, #19859, #1296, .T. ) ;
#9795 = DIRECTION ( 'NONE',  ( -0.01292394549866731843, -0.005513023399720594006, -0.9999012842304693116 ) ) ;
#9796 = CARTESIAN_POINT ( 'NONE',  ( -88.16332400514416179, 88.24736152454507021, 52.92523720185091207 ) ) ;
#9797 = ADVANCED_FACE ( 'NONE', ( #15207 ), #7941, .T. ) ;
#9798 = CARTESIAN_POINT ( 'NONE',  ( -16.82962413914983912, 177.4987173824078468, 90.66609475777795524 ) ) ;
#9799 = EDGE_CURVE ( 'NONE', #6385, #17869, #2398, .T. ) ;
#9801 = ORIENTED_EDGE ( 'NONE', *, *, #14709, .T. ) ;
#9800 = EDGE_LOOP ( 'NONE', ( #18155, #21025, #3160, #9313 ) ) ;
#9802 = CARTESIAN_POINT ( 'NONE',  ( -10.85624112972181621, 113.6998737626107641, 127.2553023597115214 ) ) ;
#9803 = LINE ( 'NONE', #16818, #11692 ) ;
#9804 = PLANE ( 'NONE',  #18794 ) ;
#9805 = CARTESIAN_POINT ( 'NONE',  ( -88.44888535621197434, 80.14369956782289250, 31.98268552584471180 ) ) ;
#9806 = DIRECTION ( 'NONE',  ( -5.440186201345738641E-18, -1.000000000000000000, -1.334940939666364181E-17 ) ) ;
#9807 = ORIENTED_EDGE ( 'NONE', *, *, #18333, .F. ) ;
#9808 = CARTESIAN_POINT ( 'NONE',  ( 51.07356891511743413, 94.48610424851698042, 82.73688480180349814 ) ) ;
#9809 = CARTESIAN_POINT ( 'NONE',  ( -57.55251350461809778, 118.9484885890504557, 172.9440730829682877 ) ) ;
#9810 = CARTESIAN_POINT ( 'NONE',  ( 20.07011326767535309, 182.6117360806082104, 317.7501157953450956 ) ) ;
#9811 = EDGE_CURVE ( 'NONE', #16990, #17793, #4697, .T. ) ;
#9812 = DIRECTION ( 'NONE',  ( 0.9999164797902015955, 2.457859219970326020E-15, -0.01292414190464043211 ) ) ;
#9813 = DIRECTION ( 'NONE',  ( 0.01292394549866738955, 0.005513023399720468239, 0.9999012842304693116 ) ) ;
#9814 = ADVANCED_FACE ( 'NONE', ( #6219 ), #18845, .T. ) ;
#9815 = DIRECTION ( 'NONE',  ( 0.000000000000000000, 0.000000000000000000, 1.000000000000000000 ) ) ;
#9816 = CARTESIAN_POINT ( 'NONE',  ( -49.99582398951009310, 170.0000000000008242, 0.6462070952329234119 ) ) ;
#9817 = DIRECTION ( 'NONE',  ( -0.9999464000778708339, -1.417269118681738834E-05, 0.01035358732233848493 ) ) ;
#9818 = VERTEX_POINT ( 'NONE', #20100 ) ;
#9819 = FACE_OUTER_BOUND ( 'NONE', #14643, .T. ) ;
#9820 = VERTEX_POINT ( 'NONE', #11626 ) ;
#9821 = CIRCLE ( 'NONE', #18615, 8.000000000000007105 ) ;
#9822 = CARTESIAN_POINT ( 'NONE',  ( 40.97857920176954849, 107.9236484503692708, 71.39008480283784763 ) ) ;
#9823 = EDGE_CURVE ( 'NONE', #17067, #17518, #11186, .T. ) ;
#9824 = ORIENTED_EDGE ( 'NONE', *, *, #8778, .F. ) ;
#9825 =( NAMED_UNIT ( * ) SI_UNIT ( $, .STERADIAN. ) SOLID_ANGLE_UNIT ( ) );
#9826 = CARTESIAN_POINT ( 'NONE',  ( -8.880679910171080493, 180.4772689128618595, 86.66430733602781800 ) ) ;
#9827 = CARTESIAN_POINT ( 'NONE',  ( 105.5454984634617972, 78.31265485325668863, -30.98643060412782546 ) ) ;
#9828 = DIRECTION ( 'NONE',  ( -7.125109674160258889E-05, 0.9999848031710252272, -0.005512562950849897447 ) ) ;
#9829 = CARTESIAN_POINT ( 'NONE',  ( 21.71998689217155487, 185.4674263880815204, 276.2600312189053966 ) ) ;
#9830 = CYLINDRICAL_SURFACE ( 'NONE', #5512, 2.000000000000001332 ) ;
#9831 = DIRECTION ( 'NONE',  ( -0.01292414190464217898, -1.902755938799531885E-22, -0.9999164797902015955 ) ) ;
#9832 = CARTESIAN_POINT ( 'NONE',  ( -40.19568481792634884, 106.9589643049705074, 71.59466866354080139 ) ) ;
#9833 = AXIS2_PLACEMENT_3D ( 'NONE', #8947, #8604, #12313 ) ;
#9834 = CARTESIAN_POINT ( 'NONE',  ( 68.71681667565957241, 71.82428002877155393, -85.89527988174788220 ) ) ;
#9835 = EDGE_CURVE ( 'NONE', #17029, #7846, #11941, .T. ) ;
#9836 = EDGE_CURVE ( 'NONE', #3588, #5713, #3498, .T. ) ;
#9837 = CYLINDRICAL_SURFACE ( 'NONE', #11111, 1.990000000000003988 ) ;
#9838 = FACE_OUTER_BOUND ( 'NONE', #8986, .T. ) ;
#9839 = ORIENTED_EDGE ( 'NONE', *, *, #3741, .T. ) ;
#9840 = DIRECTION ( 'NONE',  ( -0.01292414190463830014, 0.000000000000000000, -0.9999164797902017066 ) ) ;
#9841 = CARTESIAN_POINT ( 'NONE',  ( -14.59198460393170294, 181.0549870649192030, 311.6709863310374544 ) ) ;
#9842 = ORIENTED_EDGE ( 'NONE', *, *, #1776, .F. ) ;
#9843 = AXIS2_PLACEMENT_3D ( 'NONE', #725, #7721, #21927 ) ;
#9844 = ORIENTED_EDGE ( 'NONE', *, *, #10659, .F. ) ;
#9845 = MANIFOLD_SOLID_BREP ( 'Stock-MAS-425-1', #5595 ) ;
#9846 = CIRCLE ( 'NONE', #1782, 8.000000000000014211 ) ;
#9847 = CARTESIAN_POINT ( 'NONE',  ( -46.77184957787964237, 141.3748088146942621, 250.0790257996952164 ) ) ;
#9848 = DIRECTION ( 'NONE',  ( 2.025474946048326158E-22, -1.000000000000000000, 1.876735158486679638E-22 ) ) ;
#9849 = CARTESIAN_POINT ( 'NONE',  ( 41.22223050257357357, 121.3072273804455250, 249.0523267991708849 ) ) ;
#9850 = CARTESIAN_POINT ( 'NONE',  ( -45.96219963993937796, 168.0879242961143518, -74.15276576609245751 ) ) ;
#9851 = AXIS2_PLACEMENT_3D ( 'NONE', #9884, #8166, #15199 ) ;
#9852 = VERTEX_POINT ( 'NONE', #8283 ) ;
#9853 = CARTESIAN_POINT ( 'NONE',  ( -41.52238611146465530, 166.0448094368136935, 269.1837510020998820 ) ) ;
#9854 = CARTESIAN_POINT ( 'NONE',  ( -15.48458306684558394, 177.8487764627609238, 315.9761681140001883 ) ) ;
#9855 = EDGE_CURVE ( 'NONE', #4445, #7048, #21104, .T. ) ;
#9856 = CONICAL_SURFACE ( 'NONE', #22649, 4.999999999999990230, 1.047197551196595855 ) ;
#9857 = CYLINDRICAL_SURFACE ( 'NONE', #17325, 5.099999999999992539 ) ;
#9858 = CIRCLE ( 'NONE', #5809, 3.100000000000005418 ) ;
#9859 = CARTESIAN_POINT ( 'NONE',  ( 8.819665691964026166, 70.56130593988652322, -89.42914081817022520 ) ) ;
#9860 = DIRECTION ( 'NONE',  ( 7.125109674364534776E-05, -0.9999848031710252272, 0.005512562950849704026 ) ) ;
#9861 = VERTEX_POINT ( 'NONE', #20343 ) ;
#9862 = CARTESIAN_POINT ( 'NONE',  ( -14.54393240331080506, 147.5935422812049467, 278.9377680796226286 ) ) ;
#9863 = ORIENTED_EDGE ( 'NONE', *, *, #14997, .T. ) ;
#9864 = CARTESIAN_POINT ( 'NONE',  ( -2.067862704742604141, 69.99999999999998579, -159.9866367664322979 ) ) ;
#9865 = CARTESIAN_POINT ( 'NONE',  ( 9.755537514967961954, 142.9459895023150580, 274.8304158214364179 ) ) ;
#9866 = CARTESIAN_POINT ( 'NONE',  ( -8.967929144405097475, 186.2768650721423569, 307.3739889994579357 ) ) ;
#9867 = ORIENTED_EDGE ( 'NONE', *, *, #6245, .T. ) ;
#9868 = CONICAL_SURFACE ( 'NONE', #21219, 3.399999999999986144, 1.029744258676653201 ) ;
#9869 = DIRECTION ( 'NONE',  ( -0.01292414190464131508, -1.902755938799530474E-22, -0.9999164797902017066 ) ) ;
#9870 = PRODUCT_DEFINITION ( 'UNKNOWN', '', #9552, #15953 ) ;
#9871 = CYLINDRICAL_SURFACE ( 'NONE', #15247, 4.199999999999997513 ) ;
#9872 = ITEM_DEFINED_TRANSFORMATION ( 'NONE', 'NONE', #16233,  #6292 ) ;
#9873 = CIRCLE ( 'NONE', #12078, 11.00000000000000178 ) ;
#9874 = ORIENTED_EDGE ( 'NONE', *, *, #2654, .T. ) ;
#9875 = LINE ( 'NONE', #11713, #19874 ) ;
#9876 = DIRECTION ( 'NONE',  ( 0.01292394549866738782, 0.005513023399720468239, 0.9999012842304692006 ) ) ;
#9877 = DIRECTION ( 'NONE',  ( 0.9999164797902015955, 6.965998958219364448E-18, -0.01292414190464157182 ) ) ;
#9878 = DIRECTION ( 'NONE',  ( 0.000000000000000000, 0.000000000000000000, 1.000000000000000000 ) ) ;
#9879 = CYLINDRICAL_SURFACE ( 'NONE', #13438, 2.000000000000004885 ) ;
#9880 = CARTESIAN_POINT ( 'NONE',  ( 106.9749367633763910, 84.99999999999997158, 25.61958048976753943 ) ) ;
#9881 = LINE ( 'NONE', #4685, #4548 ) ;
#9882 = ORIENTED_EDGE ( 'NONE', *, *, #9209, .F. ) ;
#9883 = CARTESIAN_POINT ( 'NONE',  ( -16.77414143088337184, 138.3748544051812246, 249.7078392314084567 ) ) ;
#9884 = CARTESIAN_POINT ( 'NONE',  ( -90.00000000000000000, 29.00000000000000355, 8.394090934816448357E-16 ) ) ;
#9885 = ORIENTED_EDGE ( 'NONE', *, *, #7890, .T. ) ;
#9886 = DIRECTION ( 'NONE',  ( 0.009760756503428003050, -0.9999378516499564107, 0.005387065077611006073 ) ) ;
#9887 = CARTESIAN_POINT ( 'NONE',  ( -83.92517094583074311, 79.85565591775390715, 71.13418697079595177 ) ) ;
#9888 = CARTESIAN_POINT ( 'NONE',  ( 105.7941983518663136, 70.06152065884126046, 30.12648231254615894 ) ) ;
#9889 = FACE_BOUND ( 'NONE', #4154, .T. ) ;
#9890 = VECTOR ( 'NONE', #14518, 1000.000000000000114 ) ;
#9891 = EDGE_CURVE ( 'NONE', #20163, #17220, #14871, .T. ) ;
#9892 = PRESENTATION_LAYER_ASSIGNMENT (  '', '', ( #14686 ) ) ;
#9893 = DIRECTION ( 'NONE',  ( 7.125109674081160920E-05, -0.9999848031710253382, 0.005512562950849312846 ) ) ;
#9894 = CARTESIAN_POINT ( 'NONE',  ( 90.43474204040840903, 34.61572286322119396, -31.17139488068002251 ) ) ;
#9895 = VECTOR ( 'NONE', #14388, 999.9999999999998863 ) ;
#9896 = ORIENTED_EDGE ( 'NONE', *, *, #20483, .F. ) ;
#9897 = CARTESIAN_POINT ( 'NONE',  ( 5.474031775163563651, 81.44011527025983810, -97.46771346163548344 ) ) ;
#9898 = CARTESIAN_POINT ( 'NONE',  ( -2.476119979858689923, 190.7342627770796355, 256.5417576885990343 ) ) ;
#9899 = ORIENTED_EDGE ( 'NONE', *, *, #4403, .F. ) ;
#9900 = CARTESIAN_POINT ( 'NONE',  ( -55.90526550923683402, 114.1953700931303501, 163.2999869670306623 ) ) ;
#9901 = EDGE_CURVE ( 'NONE', #5655, #14473, #10103, .T. ) ;
#9902 = CARTESIAN_POINT ( 'NONE',  ( -90.11148781677563591, 87.44634235373453635, 51.12665407066659640 ) ) ;
#9903 = CARTESIAN_POINT ( 'NONE',  ( 12.78871265281718728, 167.7718460055969274, 324.4777745207641146 ) ) ;
#9904 = VECTOR ( 'NONE', #18916, 1000.000000000000227 ) ;
#9905 = ORIENTED_EDGE ( 'NONE', *, *, #16398, .F. ) ;
#9906 = AXIS2_PLACEMENT_3D ( 'NONE', #2905, #3230, #20361 ) ;
#9907 = ADVANCED_FACE ( 'NONE', ( #12419 ), #20729, .F. ) ;
#9908 = CARTESIAN_POINT ( 'NONE',  ( -74.46989193151192410, 95.80563795305937447, 80.95834026808688577 ) ) ;
#9909 = DIRECTION ( 'NONE',  ( 0.01035335185279143318, 0.005513005182356926943, 0.9999312050732649393 ) ) ;
#9910 = CARTESIAN_POINT ( 'NONE',  ( 0.000000000000000000, 20.00000000000000000, 0.000000000000000000 ) ) ;
#9911 = CARTESIAN_POINT ( 'NONE',  ( -12.81536461602102683, 326.2504838843369726, 414.3222871145668478 ) ) ;
#9912 = CARTESIAN_POINT ( 'NONE',  ( 0.000000000000000000, 18.00000000000000355, 0.000000000000000000 ) ) ;
#9913 = CARTESIAN_POINT ( 'NONE',  ( 86.24279638190516550, 74.99899999999998101, -1.114707239275309014 ) ) ;
#9914 = AXIS2_PLACEMENT_3D ( 'NONE', #17208, #12040, #20984 ) ;
#9915 = ORIENTED_EDGE ( 'NONE', *, *, #12819, .T. ) ;
#9916 = CARTESIAN_POINT ( 'NONE',  ( -51.17105351027176141, 189.4989811950858609, -90.27908403945292548 ) ) ;
#9917 = DIRECTION ( 'NONE',  ( 0.9999164797902015955, 6.965998958219364448E-18, -0.01292414190464157182 ) ) ;
#9918 = CARTESIAN_POINT ( 'NONE',  ( 92.19968689859011590, 79.04398536104956463, -28.61667231988791826 ) ) ;
#9919 = CARTESIAN_POINT ( 'NONE',  ( -40.89051693738994686, 95.45168806188145538, 82.94916985812750454 ) ) ;
#9920 = EDGE_CURVE ( 'NONE', #10082, #19973, #7160, .T. ) ;
#9921 = EDGE_CURVE ( 'NONE', #11656, #14225, #18196, .T. ) ;
#9922 = DIRECTION ( 'NONE',  ( -0.01292414190463827932, 0.000000000000000000, -0.9999164797902018176 ) ) ;
#9923 = ORIENTED_EDGE ( 'NONE', *, *, #21388, .T. ) ;
#9924 = VECTOR ( 'NONE', #3514, 999.9999999999998863 ) ;
#9925 = DIRECTION ( 'NONE',  ( 1.000000000000000000, 0.000000000000000000, -1.396592535537260757E-14 ) ) ;
#9926 = CARTESIAN_POINT ( 'NONE',  ( 153.9999999999992610, 20.00000000000000000, 53.76161406891468175 ) ) ;
#9927 = ORIENTED_EDGE ( 'NONE', *, *, #10461, .F. ) ;
#9928 = CARTESIAN_POINT ( 'NONE',  ( -146.5000000000000000, 0.000000000000000000, -9.999999999999982236 ) ) ;
#9929 = ORIENTED_EDGE ( 'NONE', *, *, #5623, .F. ) ;
#9930 = EDGE_CURVE ( 'NONE', #12065, #17671, #12317, .T. ) ;
#9931 = DIRECTION ( 'NONE',  ( -0.4397038457472429718, 0.000000000000000000, 0.8981428216242028917 ) ) ;
#9932 = CIRCLE ( 'NONE', #12872, 2.000000000000004885 ) ;
#9933 = ADVANCED_FACE ( 'NONE', ( #21020 ), #20786, .F. ) ;
#9934 = VERTEX_POINT ( 'NONE', #20677 ) ;
#9935 = ADVANCED_FACE ( 'NONE', ( #15425 ), #15649, .F. ) ;
#9936 = CARTESIAN_POINT ( 'NONE',  ( -49.84871199900936745, 107.0846990171262689, 71.28987068907396463 ) ) ;
#9937 = DIRECTION ( 'NONE',  ( -5.440186201345738641E-18, -1.000000000000000000, -1.334940939666364181E-17 ) ) ;
#9938 = AXIS2_PLACEMENT_3D ( 'NONE', #5750, #9980, #6426 ) ;
#9939 = CARTESIAN_POINT ( 'NONE',  ( -0.9693106428480922077, 72.00000000000000000, -74.99373598426512899 ) ) ;
#9940 = AXIS2_PLACEMENT_3D ( 'NONE', #21077, #9117, #1786 ) ;
#9941 = DIRECTION ( 'NONE',  ( -0.4397038457472479678, 0.000000000000000000, -0.8981428216242003382 ) ) ;
#9942 = VECTOR ( 'NONE', #7757, 1000.000000000000227 ) ;
#9943 = CYLINDRICAL_SURFACE ( 'NONE', #3644, 3.399999999999986144 ) ;
#9944 = CARTESIAN_POINT ( 'NONE',  ( 1.458023040593674057E-15, 18.00000000000000355, 9.999999999999994671 ) ) ;
#9945 = CARTESIAN_POINT ( 'NONE',  ( 63.56236266363622889, 189.3893605493459233, -111.6473409898501075 ) ) ;
#9946 = DIRECTION ( 'NONE',  ( 0.9999164797902017066, 2.001050586450177050E-22, -0.01292414190464218071 ) ) ;
#9947 = DIRECTION ( 'NONE',  ( 0.01292394549866738782, 0.005513023399720468239, 0.9999012842304692006 ) ) ;
#9948 = EDGE_CURVE ( 'NONE', #3348, #15608, #12196, .T. ) ;
#9949 = DIRECTION ( 'NONE',  ( 0.000000000000000000, 0.000000000000000000, -1.000000000000000000 ) ) ;
#9950 = EDGE_LOOP ( 'NONE', ( #14096, #14209, #15213 ) ) ;
#9951 = AXIS2_PLACEMENT_3D ( 'NONE', #14349, #19596, #10881 ) ;
#9952 = CIRCLE ( 'NONE', #43, 11.00000000000000178 ) ;
#9953 = CARTESIAN_POINT ( 'NONE',  ( 91.81287659828484493, 71.13119029400844795, 60.58394261007850901 ) ) ;
#9954 = VERTEX_POINT ( 'NONE', #10127 ) ;
#9955 = VERTEX_POINT ( 'NONE', #18950 ) ;
#9956 = CARTESIAN_POINT ( 'NONE',  ( -158.3970384574724335, 1.999999999999998224, -62.74304228515459414 ) ) ;
#9957 = DIRECTION ( 'NONE',  ( 0.009760756503427813965, -0.9999378516499565217, 0.005387065077607405654 ) ) ;
#9958 = ORIENTED_EDGE ( 'NONE', *, *, #17387, .F. ) ;
#9959 = ORIENTED_EDGE ( 'NONE', *, *, #9392, .T. ) ;
#9960 = CARTESIAN_POINT ( 'NONE',  ( 19.99832959580401948, 170.0000000000008242, -0.2584828380919867996 ) ) ;
#9961 = ORIENTED_EDGE ( 'NONE', *, *, #5120, .T. ) ;
#9962 = AXIS2_PLACEMENT_3D ( 'NONE', #22489, #8051, #4492 ) ;
#9963 =( GEOMETRIC_REPRESENTATION_CONTEXT ( 3 ) GLOBAL_UNCERTAINTY_ASSIGNED_CONTEXT ( ( #9529 ) ) GLOBAL_UNIT_ASSIGNED_CONTEXT ( ( #3784, #8827, #8945 ) ) REPRESENTATION_CONTEXT ( 'NONE', 'WORKASPACE' ) );
#9964 = MANIFOLD_SOLID_BREP ( 'Stock-MAS-425-1', #17017 ) ;
#9965 = DIRECTION ( 'NONE',  ( 0.01292414190463953873, 0.000000000000000000, 0.9999164797902017066 ) ) ;
#9966 = EDGE_CURVE ( 'NONE', #19051, #16346, #10353, .T. ) ;
#9967 = EDGE_LOOP ( 'NONE', ( #12533, #12213, #14330, #3359 ) ) ;
#9968 = DIRECTION ( 'NONE',  ( 0.01292394549866738608, 0.005513023399721785761, 0.9999012842304693116 ) ) ;
#9969 = CARTESIAN_POINT ( 'NONE',  ( 9.196690372329099361, 142.8086146031528187, 274.7267082784171066 ) ) ;
#9970 = ORIENTED_EDGE ( 'NONE', *, *, #9514, .F. ) ;
#9971 = AXIS2_PLACEMENT_3D ( 'NONE', #17004, #20406, #11480 ) ;
#9972 = VECTOR ( 'NONE', #7986, 1000.000000000000114 ) ;
#9973 = EDGE_CURVE ( 'NONE', #5484, #15351, #17243, .T. ) ;
#9974 = CARTESIAN_POINT ( 'NONE',  ( -10.90116789308776113, 162.9865723938430051, 122.9837558165935292 ) ) ;
#9975 = CARTESIAN_POINT ( 'NONE',  ( -16.68277397329964273, 181.4144828908143552, 256.7767670742539963 ) ) ;
#9976 = CARTESIAN_POINT ( 'NONE',  ( -90.43474204040838060, 72.00000000000000000, 31.17139488067998343 ) ) ;
#9977 = CONICAL_SURFACE ( 'NONE', #820, 117.0000000000000000, 0.3316125578789227979 ) ;
#9978 = CARTESIAN_POINT ( 'NONE',  ( -1.247179693797872524, 44.99899999999999523, -96.49194029975447506 ) ) ;
#9979 = EDGE_LOOP ( 'NONE', ( #2001, #7147, #13460 ) ) ;
#9980 = DIRECTION ( 'NONE',  ( 7.125109674403276030E-05, -0.9999848031710252272, 0.005512562950848280685 ) ) ;
#9981 = CARTESIAN_POINT ( 'NONE',  ( -88.74294073166163344, 70.70905333810220839, 62.85632276041776123 ) ) ;
#9982 = CONICAL_SURFACE ( 'NONE', #11086, 3.399999999999985700, 1.029744258676653201 ) ;
#9983 = LINE ( 'NONE', #11830, #2175 ) ;
#9984 = LINE ( 'NONE', #21593, #3319 ) ;
#9985 = CARTESIAN_POINT ( 'NONE',  ( -28.52776333611105386, 324.0526502209150976, 314.9593530838130278 ) ) ;
#9986 = DIRECTION ( 'NONE',  ( -7.125109674158749138E-05, 0.9999848031710253382, -0.005512562950850162860 ) ) ;
#9987 = CARTESIAN_POINT ( 'NONE',  ( -9.912705577010314703E-16, 0.000000000000000000, -9.999999999999994671 ) ) ;
#9988 = VECTOR ( 'NONE', #13860, 999.9999999999998863 ) ;
#9989 = STYLED_ITEM ( 'NONE', ( #15725 ), #17010 ) ;
#9990 = DIRECTION ( 'NONE',  ( 0.01035335185279153900, 0.005513005182355262476, 0.9999312050732647172 ) ) ;
#9991 = EDGE_CURVE ( 'NONE', #18579, #7906, #15993, .T. ) ;
#9992 = ITEM_DEFINED_TRANSFORMATION ( 'NONE', 'NONE', #20961,  #6292 ) ;
#9993 = EDGE_CURVE ( 'NONE', #15528, #564, #15760, .T. ) ;
#9994 = ORIENTED_EDGE ( 'NONE', *, *, #17663, .F. ) ;
#9995 = CARTESIAN_POINT ( 'NONE',  ( -52.56646033833638398, 109.2346207959984241, -43.48992611560825594 ) ) ;
#9996 = ORIENTED_EDGE ( 'NONE', *, *, #8797, .T. ) ;
#9997 = DIRECTION ( 'NONE',  ( -0.9999164797902017066, -2.001050586450178931E-22, 0.01292414190464131508 ) ) ;
#9998 = VECTOR ( 'NONE', #6090, 1000.000000000000000 ) ;
#9999 = CARTESIAN_POINT ( 'NONE',  ( 64.08803682720244410, 103.0000000000000000, -70.97692255680823337 ) ) ;
#10000 = CARTESIAN_POINT ( 'NONE',  ( 2.830031787867828275, 81.19615242270661781, -80.39798906481894392 ) ) ;
#10001 = DIRECTION ( 'NONE',  ( -0.9506032891036972909, 0.3102281881984321754, 0.01057629388542893900 ) ) ;
#10002 =( REPRESENTATION_RELATIONSHIP ('NONE','NONE', #11808, #17373 ) REPRESENTATION_RELATIONSHIP_WITH_TRANSFORMATION ( #10329 )SHAPE_REPRESENTATION_RELATIONSHIP( ) );
#10003 = ORIENTED_EDGE ( 'NONE', *, *, #10761, .F. ) ;
#10004 = CARTESIAN_POINT ( 'NONE',  ( -73.00030478232707765, 95.66452290628956234, 82.28581592040848136 ) ) ;
#10005 = ORIENTED_EDGE ( 'NONE', *, *, #20718, .F. ) ;
#10006 = DIRECTION ( 'NONE',  ( 1.387778780781444571E-14, -0.000000000000000000, 1.000000000000000000 ) ) ;
#10007 = DIRECTION ( 'NONE',  ( 0.8981428216242060003, 1.398976466700252608E-14, 0.4397038457472368655 ) ) ;
#10008 = CARTESIAN_POINT ( 'NONE',  ( 105.9308899693960626, 70.24357031783570449, 29.64301131075924545 ) ) ;
#10009 = CARTESIAN_POINT ( 'NONE',  ( -79.00000000000000000, 29.00000000000000355, 7.368146487227772848E-16 ) ) ;
#10010 = CIRCLE ( 'NONE', #10746, 124.0000000000000000 ) ;
#10011 = AXIS2_PLACEMENT_3D ( 'NONE', #14756, #20099, #14972 ) ;
#10012 = EDGE_LOOP ( 'NONE', ( #5274, #3903 ) ) ;
#10013 = CARTESIAN_POINT ( 'NONE',  ( 45.23671757199362986, 168.6025580852140138, 18.02358667753535926 ) ) ;
#10014 = FILL_AREA_STYLE_COLOUR ( '', #17455 ) ;
#10015 = VERTEX_POINT ( 'NONE', #9171 ) ;
#10016 = CARTESIAN_POINT ( 'NONE',  ( 7.145902869757795983, 81.99999999999998579, -93.45069977196735067 ) ) ;
#10017 = AXIS2_PLACEMENT_3D ( 'NONE', #9850, #9752, #16874 ) ;
#10018 = DIRECTION ( 'NONE',  ( 0.9909299940865188283, -0.1338359446631172955, -0.01207007604876741101 ) ) ;
#10019 = ORIENTED_EDGE ( 'NONE', *, *, #1210, .F. ) ;
#10020 = DIRECTION ( 'NONE',  ( 0.7562662552911934011, -0.5735764363510514885, -0.3147561322209044832 ) ) ;
#10021 = EDGE_CURVE ( 'NONE', #2415, #9625, #6062, .T. ) ;
#10022 = CARTESIAN_POINT ( 'NONE',  ( -90.08534597741504513, 88.53258948335707146, 52.71256580331551334 ) ) ;
#10024 = LINE ( 'NONE', #9903, #22492 ) ;
#10023 = VECTOR ( 'NONE', #21749, 1000.000000000000000 ) ;
#10025 = ORIENTED_EDGE ( 'NONE', *, *, #12368, .T. ) ;
#10026 = AXIS2_PLACEMENT_3D ( 'NONE', #8381, #2991, #15316 ) ;
#10027 = B_SPLINE_CURVE_WITH_KNOTS ( 'NONE', 3,
 ( #13741, #20608, #13410, #11787, #6716, #20488, #15253, #11903, #10279, #13844, #8425, #22206, #1555, #5086 ),
 .UNSPECIFIED., .F., .F.,
 ( 4, 2, 2, 2, 2, 2, 4 ),
 ( 0.000000000000000000, 0.001119727475084575678, 0.001679591212626860156, 0.002239454950169144417, 0.003359182425253676510, 0.003919046162795964891, 0.004478909900338253272 ),
 .UNSPECIFIED. ) ;
#10028 = CARTESIAN_POINT ( 'NONE',  ( -72.51438462527775641, 87.23323244114081376, 69.92599951943640235 ) ) ;
#10029 = CARTESIAN_POINT ( 'NONE',  ( -75.38289248423089361, 96.35610324583468866, 81.62497328870777835 ) ) ;
#10030 = CARTESIAN_POINT ( 'NONE',  ( -44.65205341519984472, 164.1467306581422179, 27.21077625607567541 ) ) ;
#10031 = DIRECTION ( 'NONE',  ( -2.025474946048326158E-22, 1.000000000000000000, -1.876735158486679638E-22 ) ) ;
#10032 = CYLINDRICAL_SURFACE ( 'NONE', #19193, 2.000000000000000000 ) ;
#10033 = CARTESIAN_POINT ( 'NONE',  ( -71.43040806848136981, 92.41825753590678971, -83.65230687350626226 ) ) ;
#10034 = VERTEX_POINT ( 'NONE', #10685 ) ;
#10035 = DIRECTION ( 'NONE',  ( 0.01292394549866728373, 0.005513023399720296501, 0.9999012842304693116 ) ) ;
#10036 = CLOSED_SHELL ( 'NONE', ( #6052, #14747, #10499, #21183, #14133, #15592, #13580, #20570, #13292, #20080, #16998, #18740, #16786, #11469, #8183, #3374, #20453, #10877, #18803, #6457, #12883, #17447, #10921, #10331, #18480, #19729, #5940, #22656, #21058, #21588, #12625, #5431, #1158, #20420, #20221, #21137, #208, #7427, #3055, #17921, #14685, #6006, #8418, #9054, #22014, #18716, #10125, #10747, #14268, #14449, #4560, #22185, #15274, #999, #2486, #16717, #6431, #811, #13201, #8367, #16730, #9459, #12620, #21997, #6585, #3524, #19709, #5983, #16146, #15765, #16110, #547, #17807, #11371, #6346, #3739, #22285, #8764, #7397, #19449, #8441, #14152, #22274, #944, #9765, #22630, #22087, #10932, #2835, #11068, #12511, #14503, #2113, #5480, #2151, #21687, #978, #18775, #15825, #4598, #10487, #5560, #19890, #12606, #7289, #21333, #1817, #7714, #14589, #21288 ) ) ;
#10037 = VECTOR ( 'NONE', #1344, 1000.000000000000000 ) ;
#10038 = LINE ( 'NONE', #6911, #3929 ) ;
#10039 = LINE ( 'NONE', #4626, #2619 ) ;
#10040 = EDGE_CURVE ( 'NONE', #20154, #13967, #7398, .T. ) ;
#10041 = CARTESIAN_POINT ( 'NONE',  ( -3.711637254857439228, 143.2701774585193277, 275.7994991500716537 ) ) ;
#10042 = CARTESIAN_POINT ( 'NONE',  ( 64.99457118636310327, 170.0000000000000284, -0.8400692238017243296 ) ) ;
#10043 = VECTOR ( 'NONE', #1978, 1000.000000000000000 ) ;
#10044 = AXIS2_PLACEMENT_3D ( 'NONE', #512, #12927, #4383 ) ;
#10045 = CARTESIAN_POINT ( 'NONE',  ( -64.02612899542262426, 99.97194305692366356, 75.76661472217124071 ) ) ;
#10046 = VERTEX_POINT ( 'NONE', #5621 ) ;
#10047 = CARTESIAN_POINT ( 'NONE',  ( -11.39723178008673443, 186.9724665881753367, 276.4227300934390996 ) ) ;
#10048 = ORIENTED_EDGE ( 'NONE', *, *, #4460, .T. ) ;
#10049 = ORIENTED_EDGE ( 'NONE', *, *, #19074, .T. ) ;
#10050 = B_SPLINE_CURVE_WITH_KNOTS ( 'NONE', 3,
 ( #9383, #18142, #15970, #7205 ),
 .UNSPECIFIED., .F., .F.,
 ( 4, 4 ),
 ( 2.380735204249574594E-07, 0.002921158035944515681 ),
 .UNSPECIFIED. ) ;
#10051 = EDGE_CURVE ( 'NONE', #7993, #22518, #8616, .T. ) ;
#10052 = LINE ( 'NONE', #1547, #175 ) ;
#10053 = VECTOR ( 'NONE', #9674, 1000.000000000000000 ) ;
#10054 = VECTOR ( 'NONE', #19284, 999.9999999999998863 ) ;
#10055 = EDGE_CURVE ( 'NONE', #20855, #16568, #15999, .T. ) ;
#10057 = VERTEX_POINT ( 'NONE', #463 ) ;
#10056 = ORIENTED_EDGE ( 'NONE', *, *, #4162, .T. ) ;
#10058 = EDGE_CURVE ( 'NONE', #21686, #2719, #3858, .T. ) ;
#10059 = CARTESIAN_POINT ( 'NONE',  ( -50.81567181550707346, 106.8152932104169537, 71.58674244103214335 ) ) ;
#10060 = DIRECTION ( 'NONE',  ( -0.008899921406766564749, 0.7251151399516315710, -0.6885701309321218266 ) ) ;
#10061 = EDGE_CURVE ( 'NONE', #17705, #19271, #6584, .T. ) ;
#10062 = CIRCLE ( 'NONE', #10430, 2.000000000000005329 ) ;
#10063 = AXIS2_PLACEMENT_3D ( 'NONE', #57, #13848, #3387 ) ;
#10064 = DIRECTION ( 'NONE',  ( 0.000000000000000000, 0.000000000000000000, 1.000000000000000000 ) ) ;
#10065 = DIRECTION ( 'NONE',  ( 0.01292394549866738782, 0.005513023399720468239, 0.9999012842304692006 ) ) ;
#10066 = CARTESIAN_POINT ( 'NONE',  ( 18.62401128910041237, 185.5621796316531231, 278.0519500310857666 ) ) ;
#10067 = DIRECTION ( 'NONE',  ( 1.458023040593674845E-16, 0.000000000000000000, 1.000000000000000000 ) ) ;
#10068 = FACE_OUTER_BOUND ( 'NONE', #6923, .T. ) ;
#10069 = DIRECTION ( 'NONE',  ( -0.01292394549866741384, -0.005513023399720269613, -0.9999012842304692006 ) ) ;
#10070 = DIRECTION ( 'NONE',  ( 5.257939330034138471E-16, 1.000000000000000000, -6.796193297819532347E-18 ) ) ;
#10071 = EDGE_CURVE ( 'NONE', #6559, #8991, #193, .T. ) ;
#10072 = VERTEX_POINT ( 'NONE', #12757 ) ;
#10073 = DIRECTION ( 'NONE',  ( 0.9999164797902015955, 0.000000000000000000, -0.01292414190463754553 ) ) ;
#10074 = TOROIDAL_SURFACE ( 'NONE', #16344, 17.29295143883736330, 7.000000000000003553 ) ;
#10075 = EDGE_CURVE ( 'NONE', #4519, #11414, #11021, .T. ) ;
#10076 = ORIENTED_EDGE ( 'NONE', *, *, #19467, .F. ) ;
#10077 = CARTESIAN_POINT ( 'NONE',  ( -39.66554348713765421, 94.53068483135839983, 83.95012769032760502 ) ) ;
#10078 = CARTESIAN_POINT ( 'NONE',  ( -11.46885069223597853, 81.99999999999998579, -91.33151364841880593 ) ) ;
#10079 = VERTEX_POINT ( 'NONE', #3996 ) ;
#10080 = TOROIDAL_SURFACE ( 'NONE', #16706, 21.67179167071591550, 2.000000000000000000 ) ;
#10081 = DIRECTION ( 'NONE',  ( 0.9999164797902015955, 6.965998958219364448E-18, -0.01292414190464157182 ) ) ;
#10082 = VERTEX_POINT ( 'NONE', #2297 ) ;
#10083 = EDGE_CURVE ( 'NONE', #5372, #16712, #9298, .T. ) ;
#10084 = DIRECTION ( 'NONE',  ( 0.9999164797902017066, 2.001050586450178931E-22, -0.01292414190464131508 ) ) ;
#10085 = EDGE_CURVE ( 'NONE', #18095, #1703, #3667, .T. ) ;
#10086 = EDGE_CURVE ( 'NONE', #3357, #3975, #18907, .T. ) ;
#10087 = CARTESIAN_POINT ( 'NONE',  ( -0.4653277981563680443, 327.2444197121904494, 310.6395216073121333 ) ) ;
#10088 = CARTESIAN_POINT ( 'NONE',  ( -9.829246957410544994, 187.6861180068510464, 321.1599766194978542 ) ) ;
#10089 = CARTESIAN_POINT ( 'NONE',  ( 10.29791149212331902, 143.0840241353079421, 275.0539025729775631 ) ) ;
#10090 = CARTESIAN_POINT ( 'NONE',  ( 13.75908793881580294, 187.5646522750408565, 320.9026951369706921 ) ) ;
#10091 = AXIS2_PLACEMENT_3D ( 'NONE', #2104, #12693, #1766 ) ;
#10092 = DIRECTION ( 'NONE',  ( 0.9250486434174662875, 0.3795887553195633202, -0.01404934683357507604 ) ) ;
#10093 = EDGE_LOOP ( 'NONE', ( #14817, #9905, #13688, #15298, #12285 ) ) ;
#10094 = CYLINDRICAL_SURFACE ( 'NONE', #12557, 2.000000000000000000 ) ;
#10095 = LINE ( 'NONE', #9976, #17425 ) ;
#10096 = ADVANCED_FACE ( 'NONE', ( #9404 ), #691, .F. ) ;
#10097 = VERTEX_POINT ( 'NONE', #9981 ) ;
#10098 = CARTESIAN_POINT ( 'NONE',  ( -10.85567112094788200, 105.6999953372425551, 127.2994028633183348 ) ) ;
#10099 = EDGE_CURVE ( 'NONE', #21379, #4157, #19267, .T. ) ;
#10100 = LINE ( 'NONE', #1705, #20160 ) ;
#10101 = DIRECTION ( 'NONE',  ( 0.7116070947332493457, 0.08419371040299269970, 0.6975147036829268954 ) ) ;
#10102 = DIRECTION ( 'NONE',  ( 0.01292394549866738608, 0.005513023399720699824, 0.9999012842304692006 ) ) ;
#10103 = CIRCLE ( 'NONE', #5681, 3.099999999999998757 ) ;
#10104 = CARTESIAN_POINT ( 'NONE',  ( 2.830031787867828275, 70.80384757729338219, -80.39798906481894392 ) ) ;
#10105 = ADVANCED_FACE ( 'NONE', ( #22235 ), #14949, .F. ) ;
#10106 = CARTESIAN_POINT ( 'NONE',  ( 49.99582398951007889, 170.0000000000000284, -0.6462070952321007367 ) ) ;
#10107 = EDGE_CURVE ( 'NONE', #9038, #18453, #924, .T. ) ;
#10108 = VERTEX_POINT ( 'NONE', #18370 ) ;
#10109 = DIRECTION ( 'NONE',  ( 0.000000000000000000, -1.000000000000000000, 0.000000000000000000 ) ) ;
#10110 = VERTEX_POINT ( 'NONE', #7913 ) ;
#10111 = FACE_OUTER_BOUND ( 'NONE', #10476, .T. ) ;
#10112 = FACE_OUTER_BOUND ( 'NONE', #19507, .T. ) ;
#10113 = VERTEX_POINT ( 'NONE', #13335 ) ;
#10114 = AXIS2_PLACEMENT_3D ( 'NONE', #16359, #11160, #598 ) ;
#10115 = CARTESIAN_POINT ( 'NONE',  ( -55.40268456415261511, 18.00000000000000355, 113.1659955246496025 ) ) ;
#10116 = PRODUCT_DEFINITION_SHAPE ( 'NONE', 'NONE',  #22693 ) ;
#10117 = CARTESIAN_POINT ( 'NONE',  ( -48.56673365018540522, 108.3817487785542824, -43.53692110109249569 ) ) ;
#10118 = ORIENTED_EDGE ( 'NONE', *, *, #12019, .F. ) ;
#10119 = CARTESIAN_POINT ( 'NONE',  ( 48.79964398845571338, 112.2287212901250228, -44.81661363440452561 ) ) ;
#10120 = EDGE_LOOP ( 'NONE', ( #988, #709, #12775, #10725 ) ) ;
#10121 = CARTESIAN_POINT ( 'NONE',  ( 157.5176307659771453, 20.00000000000000000, 60.94675664190832975 ) ) ;
#10122 = DIRECTION ( 'NONE',  ( -0.8981428216242087759, 0.000000000000000000, 0.4397038457472309259 ) ) ;
#10123 = DIRECTION ( 'NONE',  ( -0.9999164797902015955, -8.506845633049209592E-18, 0.01292414190464159611 ) ) ;
#10124 = ORIENTED_EDGE ( 'NONE', *, *, #19955, .T. ) ;
#10125 = ADVANCED_FACE ( 'NONE', ( #21894 ), #20410, .T. ) ;
#10126 = DIRECTION ( 'NONE',  ( -2.025474946048326158E-22, 1.000000000000000000, -1.876735158486679638E-22 ) ) ;
#10127 = CARTESIAN_POINT ( 'NONE',  ( -90.00000000000000000, 29.00000000000000355, 10.99999999999999289 ) ) ;
#10128 = EDGE_CURVE ( 'NONE', #15200, #5640, #10475, .T. ) ;
#10129 = ORIENTED_EDGE ( 'NONE', *, *, #19159, .T. ) ;
#10130 = CARTESIAN_POINT ( 'NONE',  ( -39.42082737383930890, 91.17157287525388654, 83.51645567887777588 ) ) ;
#10131 = LINE ( 'NONE', #20448, #2976 ) ;
#10132 = VERTEX_POINT ( 'NONE', #4667 ) ;
#10133 = AXIS2_PLACEMENT_3D ( 'NONE', #14805, #17823, #3778 ) ;
#10134 = DIRECTION ( 'NONE',  ( 0.9934404589540163366, 0.1135548637187057675, -0.01346653032742924257 ) ) ;
#10135 = CARTESIAN_POINT ( 'NONE',  ( -89.95810659785270502, 88.78972713510226811, 52.40189527015975557 ) ) ;
#10137 = ORIENTED_EDGE ( 'NONE', *, *, #15379, .T. ) ;
#10136 = ORIENTED_EDGE ( 'NONE', *, *, #18770, .T. ) ;
#10138 = APPLICATION_CONTEXT ( 'automotive_design' ) ;
#10139 = PLANE ( 'NONE',  #19492 ) ;
#10140 = CARTESIAN_POINT ( 'NONE',  ( -64.35900422130245602, 88.71869973106718987, 50.01268641288888972 ) ) ;
#10141 = DIRECTION ( 'NONE',  ( -0.01292394549866731843, -0.005513023399720594006, -0.9999012842304693116 ) ) ;
#10142 = ORIENTED_EDGE ( 'NONE', *, *, #11041, .T. ) ;
#10143 = B_SPLINE_CURVE_WITH_KNOTS ( 'NONE', 3,
 ( #19744, #9190, #16240, #21247, #12771, #13019, #5515, #11269, #7589, #4015, #11042, #2314, #19540, #9419, #17851, #16459 ),
 .UNSPECIFIED., .F., .F.,
 ( 4, 2, 2, 2, 2, 2, 2, 4 ),
 ( 0.000000000000000000, 0.0003989315947993856814, 0.0007978631895987713628, 0.001196794784398157044, 0.001595726379197542726, 0.002393589568796313221, 0.002792521163595688711, 0.003191452758395064201 ),
 .UNSPECIFIED. ) ;
#10144 = CARTESIAN_POINT ( 'NONE',  ( 49.97599159607656816, 113.1437488774104594, -44.83686325422981156 ) ) ;
#10145 = FACE_OUTER_BOUND ( 'NONE', #20183, .T. ) ;
#10146 = ORIENTED_EDGE ( 'NONE', *, *, #10316, .F. ) ;
#10147 = ORIENTED_EDGE ( 'NONE', *, *, #4777, .F. ) ;
#10148 = EDGE_LOOP ( 'NONE', ( #153, #2630, #9721, #7811 ) ) ;
#10149 = DIRECTION ( 'NONE',  ( 7.125109674364534776E-05, -0.9999848031710252272, 0.005512562950849704893 ) ) ;
#10150 = LINE ( 'NONE', #8520, #22116 ) ;
#10151 = CARTESIAN_POINT ( 'NONE',  ( 89.78684647853556555, 79.34753190266587808, -29.57356476272795121 ) ) ;
#10152 = CARTESIAN_POINT ( 'NONE',  ( 48.46580958134982353, 166.9169248112777666, 268.0158251802795917 ) ) ;
#10153 = CARTESIAN_POINT ( 'NONE',  ( -9.861378660640976790, 146.2806317597711256, 277.1079458220327183 ) ) ;
#10154 =( LENGTH_UNIT ( ) NAMED_UNIT ( * ) SI_UNIT ( .MILLI., .METRE. ) );
#10155 = LINE ( 'NONE', #22411, #9592 ) ;
#10156 = CARTESIAN_POINT ( 'NONE',  ( -10.09063251380018400, 187.4441295575114168, 321.1374866210967980 ) ) ;
#10157 = VERTEX_POINT ( 'NONE', #11597 ) ;
#10158 = ORIENTED_EDGE ( 'NONE', *, *, #4774, .F. ) ;
#10159 = CARTESIAN_POINT ( 'NONE',  ( -16.85532952795369255, 175.4877217292663545, 88.67731731521871552 ) ) ;
#10160 = ORIENTED_EDGE ( 'NONE', *, *, #9063, .T. ) ;
#10161 = DIRECTION ( 'NONE',  ( -2.449293598294706414E-16, 0.000000000000000000, -1.000000000000000000 ) ) ;
#10162 = CARTESIAN_POINT ( 'NONE',  ( -89.95770071757259245, 72.76905099204731187, 61.70965611469623013 ) ) ;
#10163 = CARTESIAN_POINT ( 'NONE',  ( 85.34197260657376205, 75.05748221035003098, 2.205900974544971138 ) ) ;
#10164 = CARTESIAN_POINT ( 'NONE',  ( -41.67747345744908216, 165.9786531560170886, 257.1849355913342379 ) ) ;
#10165 = CARTESIAN_POINT ( 'NONE',  ( 18.15246772113923512, 187.2525995768337737, 276.0409225219374321 ) ) ;
#10166 = DIRECTION ( 'NONE',  ( 1.224646799147349509E-16, 0.000000000000000000, -1.000000000000000000 ) ) ;
#10167 = CARTESIAN_POINT ( 'NONE',  ( 41.86260591032142742, 94.79175134113202716, 83.13175616242061494 ) ) ;
#10168 = FACE_OUTER_BOUND ( 'NONE', #3869, .T. ) ;
#10169 = FACE_OUTER_BOUND ( 'NONE', #22110, .T. ) ;
#10170 = ORIENTED_EDGE ( 'NONE', *, *, #2689, .F. ) ;
#10171 = CARTESIAN_POINT ( 'NONE',  ( 88.41758806590425479, 80.31838830481380853, -32.48564084813598640 ) ) ;
#10172 = ORIENTED_EDGE ( 'NONE', *, *, #3141, .T. ) ;
#10173 = FACE_OUTER_BOUND ( 'NONE', #1633, .T. ) ;
#10174 = EDGE_LOOP ( 'NONE', ( #14222, #21310, #8440, #9528, #16260, #19726, #11548, #1078, #11985, #15523, #20352, #2204 ) ) ;
#10175 = EDGE_CURVE ( 'NONE', #6510, #15210, #15290, .T. ) ;
#10176 = VERTEX_POINT ( 'NONE', #18592 ) ;
#10177 = CARTESIAN_POINT ( 'NONE',  ( -55.72733096459582924, 118.9028271686689209, 164.6374518001329363 ) ) ;
#10178 = CARTESIAN_POINT ( 'NONE',  ( -9.831917787258822372, 187.9991244538465480, 308.1409416784720179 ) ) ;
#10179 = EDGE_LOOP ( 'NONE', ( #14583, #11961, #18276, #15629, #11997, #19181, #5404, #8877, #18888 ) ) ;
#10180 = LINE ( 'NONE', #15489, #19371 ) ;
#10181 = VERTEX_POINT ( 'NONE', #8258 ) ;
#10182 = SHAPE_REPRESENTATION ( 'Moving Jaw', ( #6292 ), #11807 ) ;
#10183 = CARTESIAN_POINT ( 'NONE',  ( 1.364374644014609697E-14, 69.99999999999998579, -9.836443712999143722E-15 ) ) ;
#10184 = ADVANCED_FACE ( 'NONE', ( #16884, #2853, #1148 ), #11701, .F. ) ;
#10185 = EDGE_CURVE ( 'NONE', #20596, #11089, #15176, .T. ) ;
#10186 = PRODUCT_DEFINITION_CONTEXT ( 'detailed design', #3831, 'design' ) ;
#10187 = CARTESIAN_POINT ( 'NONE',  ( -90.00466877033377955, 70.05991977044968166, 63.23890890537643372 ) ) ;
#10189 = CIRCLE ( 'NONE', #3572, 95.00000000000001421 ) ;
#10188 = SURFACE_SIDE_STYLE ('',( #17316 ) ) ;
#10190 = CARTESIAN_POINT ( 'NONE',  ( 39.45066905836480942, 123.7663955596447352, -42.75919236024152070 ) ) ;
#10191 = EDGE_CURVE ( 'NONE', #800, #1068, #15051, .T. ) ;
#10192 = ORIENTED_EDGE ( 'NONE', *, *, #14369, .T. ) ;
#10193 = CIRCLE ( 'NONE', #5400, 110.0000000000000000 ) ;
#10194 = CARTESIAN_POINT ( 'NONE',  ( 14.46615021700412740, 189.4447416640960569, 320.6057474549900803 ) ) ;
#10195 = ORIENTED_EDGE ( 'NONE', *, *, #8893, .T. ) ;
#10196 = CARTESIAN_POINT ( 'NONE',  ( 108.7959396947362478, 76.66003400751192487, 16.85290706162241037 ) ) ;
#10197 = FILL_AREA_STYLE ('',( #3175 ) ) ;
#10198 = LINE ( 'NONE', #19367, #14112 ) ;
#10199 = VERTEX_POINT ( 'NONE', #13105 ) ;
#10200 = VECTOR ( 'NONE', #9332, 999.9999999999998863 ) ;
#10201 = EDGE_CURVE ( 'NONE', #5047, #4519, #19964, .T. ) ;
#10202 = CARTESIAN_POINT ( 'NONE',  ( 3.603563735215880026, 87.00000000000001421, -86.34855356100663926 ) ) ;
#10203 = EDGE_CURVE ( 'NONE', #3163, #4059, #8635, .T. ) ;
#10204 = CARTESIAN_POINT ( 'NONE',  ( -44.75629999235007972, 176.1024441089967638, 19.14541522682172925 ) ) ;
#10205 = CARTESIAN_POINT ( 'NONE',  ( -13.04685404786910574, 183.9066745433380845, 319.8387711160580125 ) ) ;
#10206 = EDGE_CURVE ( 'NONE', #15824, #18377, #4336, .T. ) ;
#10207 = AXIS2_PLACEMENT_3D ( 'NONE', #300, #17665, #21421 ) ;
#10208 = DIRECTION ( 'NONE',  ( 0.01292394549866731669, 0.005513023399720593139, 0.9999012842304692006 ) ) ;
#10209 = ORIENTED_EDGE ( 'NONE', *, *, #15467, .F. ) ;
#10210 = FACE_OUTER_BOUND ( 'NONE', #18589, .T. ) ;
#10211 = DIRECTION ( 'NONE',  ( 7.125109674161246868E-05, -0.9999848031710252272, 0.005512562950850154186 ) ) ;
#10212 = EDGE_CURVE ( 'NONE', #6141, #15758, #14916, .T. ) ;
#10213 = EDGE_CURVE ( 'NONE', #13377, #8239, #20074, .T. ) ;
#10214 = CONICAL_SURFACE ( 'NONE', #4324, 3.399999999999986144, 1.029744258676653201 ) ;
#10215 = ORIENTED_EDGE ( 'NONE', *, *, #18229, .T. ) ;
#10216 = LINE ( 'NONE', #8693, #6685 ) ;
#10217 = ADVANCED_FACE ( 'NONE', ( #1023, #22009 ), #8852, .F. ) ;
#10218 = DIRECTION ( 'NONE',  ( 7.125109674160325297E-05, -0.9999848031710253382, 0.005512562950849327591 ) ) ;
#10219 = DIRECTION ( 'NONE',  ( 0.9934404589540163366, 0.1135548637187051291, -0.01346653032743023830 ) ) ;
#10220 = ADVANCED_BREP_SHAPE_REPRESENTATION ( '', ( #1915, #6292 ), #7016 ) ;
#10221 = CARTESIAN_POINT ( 'NONE',  ( 48.02316444802085016, 166.7281037598372961, 233.7692061953857774 ) ) ;
#10222 = EDGE_LOOP ( 'NONE', ( #5045, #4195, #14570, #7895 ) ) ;
#10223 = CARTESIAN_POINT ( 'NONE',  ( 3.872354045398264777, 166.6517708494370709, 299.5967279023346350 ) ) ;
#10224 = DIRECTION ( 'NONE',  ( -2.025474946048326158E-22, 1.000000000000000000, -1.876735158486679638E-22 ) ) ;
#10225 = ORIENTED_EDGE ( 'NONE', *, *, #21259, .T. ) ;
#10226 = CARTESIAN_POINT ( 'NONE',  ( 50.40377811878446579, 111.4597656593367958, -47.93967249470197345 ) ) ;
#10227 = ORIENTED_EDGE ( 'NONE', *, *, #19041, .T. ) ;
#10228 =( NAMED_UNIT ( * ) SI_UNIT ( $, .STERADIAN. ) SOLID_ANGLE_UNIT ( ) );
#10229 = CARTESIAN_POINT ( 'NONE',  ( 106.2343493168401665, 77.75544475269074951, 28.53532068555786694 ) ) ;
#10230 = CARTESIAN_POINT ( 'NONE',  ( 105.6473595942261738, 69.99999999999998579, 30.63715735456338862 ) ) ;
#10231 = CARTESIAN_POINT ( 'NONE',  ( 10.98947899709743581, 165.4223666312993259, 76.48950009989302146 ) ) ;
#10232 = EDGE_CURVE ( 'NONE', #13913, #21984, #5704, .T. ) ;
#10233 = VERTEX_POINT ( 'NONE', #3224 ) ;
#10234 = DIRECTION ( 'NONE',  ( -7.125109674025824596E-05, 0.9999848031710253382, -0.005512562950849464634 ) ) ;
#10235 = EDGE_LOOP ( 'NONE', ( #21055, #2363, #4232, #7159 ) ) ;
#10236 = CARTESIAN_POINT ( 'NONE',  ( 0.000000000000000000, 18.00000000000000355, 0.000000000000000000 ) ) ;
#10237 = CARTESIAN_POINT ( 'NONE',  ( -90.02055463237803679, 34.61572286322119396, 63.21629334023816682 ) ) ;
#10238 = STYLED_ITEM ( 'NONE', ( #15432 ), #2374 ) ;
#10239 = ORIENTED_EDGE ( 'NONE', *, *, #15059, .F. ) ;
#10240 = CARTESIAN_POINT ( 'NONE',  ( 91.23431456517670313, 70.15875158948053070, -61.45272182677553729 ) ) ;
#10241 = CARTESIAN_POINT ( 'NONE',  ( -88.16520156323190349, 88.42903772351857583, 52.76279105450071683 ) ) ;
#10242 = ORIENTED_EDGE ( 'NONE', *, *, #7682, .T. ) ;
#10243 = ADVANCED_FACE ( 'NONE', ( #17385 ), #3571, .T. ) ;
#10244 = EDGE_LOOP ( 'NONE', ( #17095, #139, #13900, #7421 ) ) ;
#10245 = CARTESIAN_POINT ( 'NONE',  ( 3.086109933851330151E-14, 18.00000000000000355, 126.0000000000000000 ) ) ;
#10246 = DIRECTION ( 'NONE',  ( 5.257939330034138471E-16, 1.000000000000000000, -6.796193297819532347E-18 ) ) ;
#10247 = VERTEX_POINT ( 'NONE', #5058 ) ;
#10248 =( NAMED_UNIT ( * ) PLANE_ANGLE_UNIT ( ) SI_UNIT ( $, .RADIAN. ) );
#10249 = AXIS2_PLACEMENT_3D ( 'NONE', #6154, #2720, #12827 ) ;
#10250 = DIRECTION ( 'NONE',  ( 0.9934404589540164476, 0.1135548637187057258, -0.01346653032743022095 ) ) ;
#10251 = FACE_OUTER_BOUND ( 'NONE', #10222, .T. ) ;
#10252 = ORIENTED_EDGE ( 'NONE', *, *, #13573, .T. ) ;
#10253 = ORIENTED_EDGE ( 'NONE', *, *, #7356, .T. ) ;
#10254 = VECTOR ( 'NONE', #16565, 1000.000000000000114 ) ;
#10255 = LINE ( 'NONE', #13930, #17697 ) ;
#10256 = CARTESIAN_POINT ( 'NONE',  ( 48.31072223536619958, 166.8507685304810764, 256.0170097695137201 ) ) ;
#10257 = FACE_OUTER_BOUND ( 'NONE', #6272, .T. ) ;
#10258 = DIRECTION ( 'NONE',  ( 0.9999164797902017066, 2.001050586450178931E-22, -0.01292414190464131508 ) ) ;
#10259 = CARTESIAN_POINT ( 'NONE',  ( -11.00886142849121185, 145.7945275248869734, 276.6464210441237697 ) ) ;
#10260 = EDGE_CURVE ( 'NONE', #5580, #20892, #14171, .T. ) ;
#10261 = ORIENTED_EDGE ( 'NONE', *, *, #14466, .F. ) ;
#10262 = CARTESIAN_POINT ( 'NONE',  ( 0.000000000000000000, 0.000000000000000000, 0.000000000000000000 ) ) ;
#10263 = DIRECTION ( 'NONE',  ( -0.9999164797902017066, 0.000000000000000000, 0.01292414190463972781 ) ) ;
#10264 = CARTESIAN_POINT ( 'NONE',  ( -9.959129957705535219, 187.5668473393425302, 321.1510774957479839 ) ) ;
#10265 = ORIENTED_EDGE ( 'NONE', *, *, #2473, .F. ) ;
#10266 = ORIENTED_EDGE ( 'NONE', *, *, #4435, .F. ) ;
#10267 = AXIS2_PLACEMENT_3D ( 'NONE', #15724, #20936, #20977 ) ;
#10268 = EDGE_LOOP ( 'NONE', ( #19543, #12624, #8885, #21229 ) ) ;
#10269 = CARTESIAN_POINT ( 'NONE',  ( 51.99565694909048830, 170.0000000000000284, -0.6720553790413839046 ) ) ;
#10270 = VECTOR ( 'NONE', #9652, 1000.000000000000000 ) ;
#10271 = EDGE_LOOP ( 'NONE', ( #12710, #1281, #9268, #13133, #14861 ) ) ;
#10272 = EDGE_CURVE ( 'NONE', #7858, #1703, #10372, .T. ) ;
#10273 = AXIS2_PLACEMENT_3D ( 'NONE', #7312, #12627, #16420 ) ;
#10274 = CARTESIAN_POINT ( 'NONE',  ( -50.94642088777899147, 106.8060942374654871, 71.59769907143252965 ) ) ;
#10275 = VECTOR ( 'NONE', #8822, 1000.000000000000114 ) ;
#10276 = CARTESIAN_POINT ( 'NONE',  ( -88.26117087638380099, 71.62891547111030377, 62.33105731329421673 ) ) ;
#10277 = EDGE_CURVE ( 'NONE', #899, #20716, #7408, .T. ) ;
#10278 = CARTESIAN_POINT ( 'NONE',  ( 82.83339755747347510, 75.16617595114340133, 4.548589192762809041 ) ) ;
#10279 = CARTESIAN_POINT ( 'NONE',  ( -92.03665420188171709, 70.73625599351603910, -60.24390366714261802 ) ) ;
#10280 = EDGE_LOOP ( 'NONE', ( #2030, #6706, #4524, #13031 ) ) ;
#10281 = DIRECTION ( 'NONE',  ( -0.01292394549866632963, -0.005513023399716958026, -0.9999012842304692006 ) ) ;
#10282 = DIRECTION ( 'NONE',  ( -0.9999164797902015955, -2.001050586450181282E-22, 0.01292414190463992731 ) ) ;
#10283 = CARTESIAN_POINT ( 'NONE',  ( -0.9693106428480923187, 86.14745084375785211, -74.99373598426512899 ) ) ;
#10284 = DIRECTION ( 'NONE',  ( 0.9999164797902017066, 6.965998958219367529E-18, -0.01292414190464157182 ) ) ;
#10285 = DIRECTION ( 'NONE',  ( -0.9934404589540162256, -0.1135548637187071275, 0.01346653032743056616 ) ) ;
#10286 = CONICAL_SURFACE ( 'NONE', #7336, 3.399999999999991918, 1.029744258676652313 ) ;
#10287 = CIRCLE ( 'NONE', #2581, 2.000000000000000000 ) ;
#10288 = CARTESIAN_POINT ( 'NONE',  ( 88.44788333809653125, 80.14655074237849419, -31.99095626761635458 ) ) ;
#10289 = ORIENTED_EDGE ( 'NONE', *, *, #7129, .F. ) ;
#10290 = AXIS2_PLACEMENT_3D ( 'NONE', #9613, #11329, #14682 ) ;
#10291 = CARTESIAN_POINT ( 'NONE',  ( 19.44162203263909205, 137.6150987469609674, 111.4192551360846863 ) ) ;
#10292 = CIRCLE ( 'NONE', #17286, 3.099999999999998757 ) ;
#10293 = CARTESIAN_POINT ( 'NONE',  ( -54.52327687265812983, 0.000000000000000000, 111.3697098814011923 ) ) ;
#10294 = VERTEX_POINT ( 'NONE', #16014 ) ;
#10295 = CARTESIAN_POINT ( 'NONE',  ( -3.188732955586827789, 189.9484169693729996, 274.9698304375367002 ) ) ;
#10296 = ORIENTED_EDGE ( 'NONE', *, *, #7649, .F. ) ;
#10297 = AXIS2_PLACEMENT_3D ( 'NONE', #14634, #2851, #7599 ) ;
#10298 = VECTOR ( 'NONE', #13881, 1000.000000000000000 ) ;
#10299 = EDGE_CURVE ( 'NONE', #13257, #165, #6807, .T. ) ;
#10300 = DIRECTION ( 'NONE',  ( 0.000000000000000000, -0.000000000000000000, 1.000000000000000000 ) ) ;
#10301 = VECTOR ( 'NONE', #331, 1000.000000000000000 ) ;
#10302 = CONICAL_SURFACE ( 'NONE', #2920, 2.499999999999988010, 1.029744258676651425 ) ;
#10303 = DIRECTION ( 'NONE',  ( 7.125109674161238737E-05, -0.9999848031710253382, 0.005512562950850163727 ) ) ;
#10304 = CARTESIAN_POINT ( 'NONE',  ( 20.28499202003862223, 148.9504299946315768, 278.4103093398852025 ) ) ;
#10305 = AXIS2_PLACEMENT_3D ( 'NONE', #7201, #3758, #10771 ) ;
#10306 = ORIENTED_EDGE ( 'NONE', *, *, #8689, .T. ) ;
#10307 = CARTESIAN_POINT ( 'NONE',  ( 13.00038704669623613, 187.9860038210169364, 320.9566775397975107 ) ) ;
#10308 = ORIENTED_EDGE ( 'NONE', *, *, #22655, .F. ) ;
#10309 = CYLINDRICAL_SURFACE ( 'NONE', #1280, 85.00000000000002842 ) ;
#10310 = DIRECTION ( 'NONE',  ( -0.3796287383013209893, 0.9251388995215469313, -0.0001940304313831180127 ) ) ;
#10311 = CARTESIAN_POINT ( 'NONE',  ( 108.2112308668079521, 76.78797451630624948, -19.89137302265093510 ) ) ;
#10312 = LINE ( 'NONE', #1702, #167 ) ;
#10313 = VERTEX_POINT ( 'NONE', #14402 ) ;
#10314 = CARTESIAN_POINT ( 'NONE',  ( 12.78872557676268507, 167.7718515186203092, 324.4787744220483887 ) ) ;
#10315 = CIRCLE ( 'NONE', #15849, 97.00000000000005684 ) ;
#10316 = EDGE_CURVE ( 'NONE', #1571, #9213, #18560, .T. ) ;
#10317 = EDGE_LOOP ( 'NONE', ( #18971, #20750 ) ) ;
#10318 = DIRECTION ( 'NONE',  ( -0.01292414190464131335, -1.902755938799530239E-22, -0.9999164797902015955 ) ) ;
#10319 = CIRCLE ( 'NONE', #3700, 10.29357798165139393 ) ;
#10320 = CARTESIAN_POINT ( 'NONE',  ( 45.34064351920852687, 161.1467762486290951, 26.06414117351048176 ) ) ;
#10321 = AXIS2_PLACEMENT_3D ( 'NONE', #14995, #21947, #6244 ) ;
#10322 = CARTESIAN_POINT ( 'NONE',  ( 16.40873467035000033, 185.6567299720572635, 322.3321779654820602 ) ) ;
#10323 = AXIS2_PLACEMENT_3D ( 'NONE', #980, #18550, #2808 ) ;
#10324 = DIRECTION ( 'NONE',  ( 0.9999164797902017066, 6.965998958219365988E-18, -0.01292414190464157356 ) ) ;
#10325 = VERTEX_POINT ( 'NONE', #21577 ) ;
#10326 = PLANE ( 'NONE',  #7862 ) ;
#10327 = CARTESIAN_POINT ( 'NONE',  ( -66.18268079339598842, 69.99999999999998579, 87.86269266872857031 ) ) ;
#10328 = CARTESIAN_POINT ( 'NONE',  ( 14.04531128256715888, 105.6586476617446380, 119.4770396839737714 ) ) ;
#10329 = ITEM_DEFINED_TRANSFORMATION ( 'NONE', 'NONE', #5886,  #6292 ) ;
#10330 = CARTESIAN_POINT ( 'NONE',  ( 18.32483708604867090, 59.11803865240458578, -129.7334415360379580 ) ) ;
#10331 = ADVANCED_FACE ( 'NONE', ( #16579 ), #17953, .F. ) ;
#10332 = VERTEX_POINT ( 'NONE', #829 ) ;
#10333 = EDGE_CURVE ( 'NONE', #7846, #15942, #19635, .T. ) ;
#10334 = VECTOR ( 'NONE', #17162, 999.9999999999998863 ) ;
#10335 = ADVANCED_FACE ( 'NONE', ( #2539 ), #7481, .F. ) ;
#10336 = CYLINDRICAL_SURFACE ( 'NONE', #14789, 112.5000000000000142 ) ;
#10337 = LINE ( 'NONE', #20660, #20295 ) ;
#10338 = LINE ( 'NONE', #1607, #14780 ) ;
#10339 = LINE ( 'NONE', #6766, #14436 ) ;
#10340 = CIRCLE ( 'NONE', #5555, 9.999999999999998224 ) ;
#10341 = ORIENTED_EDGE ( 'NONE', *, *, #20033, .F. ) ;
#10342 = CARTESIAN_POINT ( 'NONE',  ( -88.18357261921191537, 87.01242838177741135, 51.36472028516209321 ) ) ;
#10343 = DIRECTION ( 'NONE',  ( 7.125109674364534776E-05, -0.9999848031710252272, 0.005512562950849704893 ) ) ;
#10344 = EDGE_LOOP ( 'NONE', ( #10775, #13525, #15958, #20905 ) ) ;
#10345 = CARTESIAN_POINT ( 'NONE',  ( 50.79682535782767161, 111.7699698251880420, -48.05900560362714202 ) ) ;
#10346 = AXIS2_PLACEMENT_3D ( 'NONE', #15848, #13771, #1811 ) ;
#10347 = VERTEX_POINT ( 'NONE', #10928 ) ;
#10348 = DIRECTION ( 'NONE',  ( 0.01292394549866738782, 0.005513023399720468239, 0.9999012842304692006 ) ) ;
#10349 = LINE ( 'NONE', #18613, #5776 ) ;
#10350 = FACE_OUTER_BOUND ( 'NONE', #19770, .T. ) ;
#10351 = ADVANCED_FACE ( 'NONE', ( #9068 ), #9314, .T. ) ;
#10352 = CARTESIAN_POINT ( 'NONE',  ( 84.66199002107499894, 104.7463091522047733, -70.23140500867290825 ) ) ;
#10353 = LINE ( 'NONE', #19179, #17084 ) ;
#10354 = EDGE_CURVE ( 'NONE', #17225, #4965, #5739, .T. ) ;
#10355 = CIRCLE ( 'NONE', #9620, 96.00000000000000000 ) ;
#10356 = ORIENTED_EDGE ( 'NONE', *, *, #15664, .F. ) ;
#10357 = AXIS2_PLACEMENT_3D ( 'NONE', #2620, #14592, #16324 ) ;
#10358 = CARTESIAN_POINT ( 'NONE',  ( -5.649437442796671149, 326.6907401307370264, 320.3464590174583577 ) ) ;
#10359 = EDGE_CURVE ( 'NONE', #19209, #9134, #9000, .T. ) ;
#10360 = ORIENTED_EDGE ( 'NONE', *, *, #15886, .T. ) ;
#10361 = CARTESIAN_POINT ( 'NONE',  ( -79.99331838321612054, 55.00000000000000000, 1.033931352371344481 ) ) ;
#10362 = CARTESIAN_POINT ( 'NONE',  ( -90.13526681931318763, 87.35670873163414285, 51.18135378728248952 ) ) ;
#10363 = AXIS2_PLACEMENT_3D ( 'NONE', #5737, #17728, #21363 ) ;
#10364 = CARTESIAN_POINT ( 'NONE',  ( -7.930164461608248607E-16, 1.999999999999998224, -7.999999999999994671 ) ) ;
#10365 = VERTEX_POINT ( 'NONE', #2431 ) ;
#10366 = EDGE_CURVE ( 'NONE', #10110, #15997, #21820, .T. ) ;
#10367 = EDGE_CURVE ( 'NONE', #8624, #5449, #17843, .T. ) ;
#10368 = ORIENTED_EDGE ( 'NONE', *, *, #4507, .T. ) ;
#10369 = CARTESIAN_POINT ( 'NONE',  ( -12.01575389183062192, 182.4076787623453129, 322.7174846376778987 ) ) ;
#10370 = DIRECTION ( 'NONE',  ( -0.01292414190463830014, 0.000000000000000000, -0.9999164797902017066 ) ) ;
#10371 = CIRCLE ( 'NONE', #8512, 10.00000000000000000 ) ;
#10372 = LINE ( 'NONE', #11983, #6074 ) ;
#10373 = TOROIDAL_SURFACE ( 'NONE', #14054, 4.000000000000000000, 2.000000000000000000 ) ;
#10374 = CARTESIAN_POINT ( 'NONE',  ( 90.43474204040840903, 72.00000000000000000, -31.17139488068002251 ) ) ;
#10375 = ORIENTED_EDGE ( 'NONE', *, *, #7786, .T. ) ;
#10376 = EDGE_LOOP ( 'NONE', ( #17336, #757, #12843, #18455 ) ) ;
#10377 = CARTESIAN_POINT ( 'NONE',  ( -13.08247124652811699, 184.1232080902636596, 278.6476637016128279 ) ) ;
#10378 = DIRECTION ( 'NONE',  ( 0.01292394549866733404, 0.005513023399720420534, 0.9999012842304693116 ) ) ;
#10379 = CARTESIAN_POINT ( 'NONE',  ( 88.83250513209151222, 79.73807450349755754, -30.77911165157509643 ) ) ;
#10380 = DIRECTION ( 'NONE',  ( -0.01292414190463827932, 0.000000000000000000, -0.9999164797902018176 ) ) ;
#10381 = CARTESIAN_POINT ( 'NONE',  ( 0.000000000000000000, 20.00000000000000000, 0.000000000000000000 ) ) ;
#10382 = DIRECTION ( 'NONE',  ( 1.000000000000000000, 0.000000000000000000, 0.000000000000000000 ) ) ;
#10383 = AXIS2_PLACEMENT_3D ( 'NONE', #19712, #3543, #17580 ) ;
#10384 = CARTESIAN_POINT ( 'NONE',  ( 105.1935855565140088, 70.39579207655377502, -32.16088115703477968 ) ) ;
#10385 = EDGE_CURVE ( 'NONE', #21648, #16549, #10143, .T. ) ;
#10386 = CARTESIAN_POINT ( 'NONE',  ( -63.99469827093767549, 99.63525711781676364, 78.19835058642853198 ) ) ;
#10387 = VERTEX_POINT ( 'NONE', #4132 ) ;
#10388 = AXIS2_PLACEMENT_3D ( 'NONE', #12851, #3773, #11004 ) ;
#10389 = ORIENTED_EDGE ( 'NONE', *, *, #9526, .F. ) ;
#10390 = CIRCLE ( 'NONE', #16287, 3.399999999999985700 ) ;
#10391 = DIRECTION ( 'NONE',  ( -0.01292414190463832269, 0.000000000000000000, -0.9999164797902017066 ) ) ;
#10392 = EDGE_LOOP ( 'NONE', ( #15066, #3338, #17673, #1022 ) ) ;
#10393 = EDGE_CURVE ( 'NONE', #8741, #5504, #21471, .T. ) ;
#10394 = LINE ( 'NONE', #5203, #3971 ) ;
#10395 = CARTESIAN_POINT ( 'NONE',  ( -39.99665919160808869, 170.0000000000000284, 0.5169656761856410432 ) ) ;
#10396 = DIRECTION ( 'NONE',  ( -2.025474946048326158E-22, 1.000000000000000000, -1.876735158486679638E-22 ) ) ;
#10397 = DIRECTION ( 'NONE',  ( 0.7944560844389304544, 0.000000000000000000, 0.6073216033519334145 ) ) ;
#10398 = LINE ( 'NONE', #4641, #3788 ) ;
#10399 = FILL_AREA_STYLE_COLOUR ( '', #3998 ) ;
#10400 = CARTESIAN_POINT ( 'NONE',  ( -40.58168163415708563, 127.0293918815982011, 187.3786108412739395 ) ) ;
#10401 = CARTESIAN_POINT ( 'NONE',  ( 11.98344425196071761, 187.6955325895518172, 304.8869668606459413 ) ) ;
#10402 = DIRECTION ( 'NONE',  ( 0.5089394657577704928, 0.004781488884709768523, 0.8607890319690653103 ) ) ;
#10403 = AXIS2_PLACEMENT_3D ( 'NONE', #20240, #4503, #20696 ) ;
#10404 = CARTESIAN_POINT ( 'NONE',  ( 90.51365344713448735, 78.00107869518899406, -32.54507930669857529 ) ) ;
#10405 =( NAMED_UNIT ( * ) PLANE_ANGLE_UNIT ( ) SI_UNIT ( $, .RADIAN. ) );
#10406 = ADVANCED_FACE ( 'NONE', ( #707 ), #19980, .T. ) ;
#10407 = CARTESIAN_POINT ( 'NONE',  ( -37.89192165770759146, 95.21750359067902991, 84.54365134533595949 ) ) ;
#10408 = CARTESIAN_POINT ( 'NONE',  ( -10.01298669457304769, 187.8806077181497471, 308.1592502570636043 ) ) ;
#10409 = EDGE_CURVE ( 'NONE', #8789, #3455, #10826, .T. ) ;
#10410 = ORIENTED_EDGE ( 'NONE', *, *, #17667, .F. ) ;
#10411 = CIRCLE ( 'NONE', #18475, 2.272904689641356502 ) ;
#10412 = AXIS2_PLACEMENT_3D ( 'NONE', #16725, #867, #16491 ) ;
#10413 = DIRECTION ( 'NONE',  ( 0.01292414190464131335, 0.000000000000000000, 0.9999164797902017066 ) ) ;
#10414 = ORIENTED_EDGE ( 'NONE', *, *, #8631, .F. ) ;
#10415 = CIRCLE ( 'NONE', #9709, 4.199999999999997513 ) ;
#10416 = CARTESIAN_POINT ( 'NONE',  ( -5.783615788470239494, 70.35631045439365039, -81.51717177438210626 ) ) ;
#10417 = ORIENTED_EDGE ( 'NONE', *, *, #20310, .F. ) ;
#10418 = DIRECTION ( 'NONE',  ( -0.01292414190464115722, 0.000000000000000000, -0.9999164797902015955 ) ) ;
#10419 = DIRECTION ( 'NONE',  ( -0.000000000000000000, -1.000000000000000000, -0.000000000000000000 ) ) ;
#10420 = CARTESIAN_POINT ( 'NONE',  ( 16.21892470842417922, 145.8010130985019828, 277.5108439706665422 ) ) ;
#10421 = EDGE_LOOP ( 'NONE', ( #801, #16859, #4877, #11211 ) ) ;
#10422 = CARTESIAN_POINT ( 'NONE',  ( 15.14365798081738745, 186.6008537337700659, 320.6317565638801739 ) ) ;
#10423 = ORIENTED_EDGE ( 'NONE', *, *, #21843, .F. ) ;
#10424 = VECTOR ( 'NONE', #10489, 1000.000000000000000 ) ;
#10425 = CARTESIAN_POINT ( 'NONE',  ( 58.09936094630035797, 143.2573102595451928, 45.99984121742717491 ) ) ;
#10426 = B_SPLINE_CURVE_WITH_KNOTS ( 'NONE', 3,
 ( #16154, #3712, #21500, #14310, #10611, #4048, #19773, #10734, #1887, #14430, #48, #2220, #1771, #11073, #8996, #15927, #8751, #15806, #21393, #10953 ),
 .UNSPECIFIED., .F., .F.,
 ( 4, 2, 2, 2, 2, 2, 2, 2, 2, 4 ),
 ( 0.000000000000000000, 0.001733977894910850113, 0.003467955789821700226, 0.005201933684732550772, 0.006935911579643400451, 0.01040386736946519522, 0.01213784526437610735, 0.01300483421183156428, 0.01343832868555929101, 0.01387182315928701948 ),
 .UNSPECIFIED. ) ;
#10427 = CYLINDRICAL_SURFACE ( 'NONE', #363, 7.500000000000002665 ) ;
#10428 = CARTESIAN_POINT ( 'NONE',  ( -10.88750796510623076, 109.6831336666334380, 124.2300622640541548 ) ) ;
#10429 = CARTESIAN_POINT ( 'NONE',  ( -56.11381622223437660, 118.5884715842524315, 107.6180086640604543 ) ) ;
#10430 = AXIS2_PLACEMENT_3D ( 'NONE', #1699, #11616, #15609 ) ;
#10431 = EDGE_LOOP ( 'NONE', ( #7586, #12006, #21426, #15879, #16956 ) ) ;
#10432 = LINE ( 'NONE', #20982, #11783 ) ;
#10433 = VECTOR ( 'NONE', #6816, 999.9999999999998863 ) ;
#10434 = EDGE_CURVE ( 'NONE', #4475, #14389, #21913, .T. ) ;
#10435 = ORIENTED_EDGE ( 'NONE', *, *, #10055, .T. ) ;
#10436 = DIRECTION ( 'NONE',  ( -0.8909995034498461308, -2.656742962652179567E-22, -0.4540042784513463880 ) ) ;
#10437 = DIRECTION ( 'NONE',  ( 0.9909299940865186063, -0.1338359446631180727, -0.01207007604876311237 ) ) ;
#10438 = CARTESIAN_POINT ( 'NONE',  ( 14.26037014339171272, 186.6883954841667332, 305.3605431179787502 ) ) ;
#10439 = DIRECTION ( 'NONE',  ( -0.009760756503427833047, 0.9999378516499565217, -0.005387065077611117095 ) ) ;
#10440 = TOROIDAL_SURFACE ( 'NONE', #545, 10.00000000000000355, 2.000000000000000000 ) ;
#10441 = DIRECTION ( 'NONE',  ( -0.004263634442766563518, 0.9440169652124856814, -0.3298693541575922761 ) ) ;
#10442 = CARTESIAN_POINT ( 'NONE',  ( 0.000000000000000000, 25.00000000000000000, 117.0000000000000000 ) ) ;
#10443 = CARTESIAN_POINT ( 'NONE',  ( 0.000000000000000000, 25.00000000000000000, 117.0000000000000000 ) ) ;
#10444 = FACE_OUTER_BOUND ( 'NONE', #12490, .T. ) ;
#10445 = VERTEX_POINT ( 'NONE', #18712 ) ;
#10446 = AXIS2_PLACEMENT_3D ( 'NONE', #20760, #14127, #10439 ) ;
#10447 = CARTESIAN_POINT ( 'NONE',  ( 21.11966452740471567, 140.4778767860209143, 86.49708559692257381 ) ) ;
#10448 = CARTESIAN_POINT ( 'NONE',  ( -10.57022244108635256, 335.9790600926598927, 330.7543525966221409 ) ) ;
#10449 = CARTESIAN_POINT ( 'NONE',  ( -54.52327687265812273, 20.00000000000000000, 111.3697098814011923 ) ) ;
#10450 = VERTEX_POINT ( 'NONE', #13233 ) ;
#10451 = DIRECTION ( 'NONE',  ( 0.000000000000000000, 1.000000000000000000, -0.000000000000000000 ) ) ;
#10452 = DIRECTION ( 'NONE',  ( 0.9934404589540162256, 0.1135548637187056842, -0.01346653032743081423 ) ) ;
#10453 = ORIENTED_EDGE ( 'NONE', *, *, #1551, .F. ) ;
#10454 = CARTESIAN_POINT ( 'NONE',  ( 50.25207249572593327, 113.2682921568431595, -44.84111833878783671 ) ) ;
#10455 = ORIENTED_EDGE ( 'NONE', *, *, #16059, .T. ) ;
#10456 = DIRECTION ( 'NONE',  ( 5.440186201345785633E-18, 1.000000000000000000, 1.334940939666367878E-17 ) ) ;
#10457 = CARTESIAN_POINT ( 'NONE',  ( 106.3114127004272689, 78.31407127224935039, 28.24702759725663270 ) ) ;
#10458 = VECTOR ( 'NONE', #721, 1000.000000000000000 ) ;
#10459 = CARTESIAN_POINT ( 'NONE',  ( 105.4334892372614405, 72.00000000000000000, -31.36525700924962834 ) ) ;
#10460 = DIRECTION ( 'NONE',  ( 0.4654428868037304712, -0.8850574712643681785, -0.006015952371159197752 ) ) ;
#10461 = EDGE_CURVE ( 'NONE', #19256, #11124, #10856, .T. ) ;
#10462 = ORIENTED_EDGE ( 'NONE', *, *, #5547, .F. ) ;
#10463 = CARTESIAN_POINT ( 'NONE',  ( 84.25113090574824071, 104.9515410254813759, -70.72375658096314055 ) ) ;
#10464 = DIRECTION ( 'NONE',  ( -1.000000000000000000, 0.000000000000000000, 1.458023040593674599E-16 ) ) ;
#10465 = ADVANCED_FACE ( 'NONE', ( #942 ), #16385, .T. ) ;
#10466 = ORIENTED_EDGE ( 'NONE', *, *, #16391, .T. ) ;
#10467 = CARTESIAN_POINT ( 'NONE',  ( 20.23006072118110055, 168.5643786070652652, 309.9923577776485217 ) ) ;
#10468 = EDGE_CURVE ( 'NONE', #495, #591, #8289, .T. ) ;
#10469 = ORIENTED_EDGE ( 'NONE', *, *, #17387, .T. ) ;
#10470 = B_SPLINE_CURVE_WITH_KNOTS ( 'NONE', 3,
 ( #3041, #15470, #17078, #18561, #6715, #2819, #9827, #16845, #8100, #18660, #15136, #22085, #13408, #20379, #8752, #14201 ),
 .UNSPECIFIED., .F., .F.,
 ( 4, 2, 2, 2, 2, 2, 2, 4 ),
 ( 0.000000000000000000, 0.0004728798714925855047, 0.0009457597429851710095, 0.001418639614477756623, 0.001891519485970342019, 0.002364399357462927415, 0.002837279228955513245, 0.003783038971940663221 ),
 .UNSPECIFIED. ) ;
#10471 = B_SPLINE_CURVE_WITH_KNOTS ( 'NONE', 3,
 ( #18148, #16533, #786, #7782, #18343, #2617, #9629 ),
 .UNSPECIFIED., .F., .F.,
 ( 4, 3, 4 ),
 ( 3.399349888776295571E-17, 0.004000000000097216589, 0.01315492597274157613 ),
 .UNSPECIFIED. ) ;
#10472 = DIRECTION ( 'NONE',  ( 0.000000000000000000, 0.000000000000000000, -1.000000000000000000 ) ) ;
#10473 = CARTESIAN_POINT ( 'NONE',  ( -88.16724451997782808, 88.59287701227550826, 52.57531193446310880 ) ) ;
#10474 = DIRECTION ( 'NONE',  ( -0.9999164797902015955, -2.001050586450178695E-22, 0.01292414190464131335 ) ) ;
#10475 = CIRCLE ( 'NONE', #9366, 2.499999999999988010 ) ;
#10476 = EDGE_LOOP ( 'NONE', ( #6204, #5874, #22317, #13064 ) ) ;
#10477 = ADVANCED_FACE ( 'NONE', ( #18391 ), #11219, .T. ) ;
#10478 = ORIENTED_EDGE ( 'NONE', *, *, #6918, .T. ) ;
#10479 = CARTESIAN_POINT ( 'NONE',  ( 54.52327687265663769, 18.00000000000000355, 111.3697098814019171 ) ) ;
#10480 = EDGE_CURVE ( 'NONE', #1302, #10046, #22148, .T. ) ;
#10481 = DIRECTION ( 'NONE',  ( 0.9999164797902017066, 2.001050586450181517E-22, -0.01292414190463992731 ) ) ;
#10482 = SURFACE_STYLE_USAGE ( .BOTH. , #8511 ) ;
#10483 = DIRECTION ( 'NONE',  ( 0.009760756503427210282, -0.9999378516499566327, 0.005387065077606872227 ) ) ;
#10484 = CARTESIAN_POINT ( 'NONE',  ( 85.08844994865407330, 75.00000638978997358, -1.434341340840276091 ) ) ;
#10485 = CARTESIAN_POINT ( 'NONE',  ( 19.44162203263909205, 137.6150987469609674, 111.4192551360846863 ) ) ;
#10486 = ORIENTED_EDGE ( 'NONE', *, *, #9579, .F. ) ;
#10487 = ADVANCED_FACE ( 'NONE', ( #21803 ), #4605, .F. ) ;
#10488 = VERTEX_POINT ( 'NONE', #20540 ) ;
#10489 = DIRECTION ( 'NONE',  ( -0.000000000000000000, -1.000000000000000000, -0.000000000000000000 ) ) ;
#10490 = CARTESIAN_POINT ( 'NONE',  ( -76.93671954797112278, 75.08645580250139062, -3.062200394342287080 ) ) ;
#10491 = CARTESIAN_POINT ( 'NONE',  ( -11.91376962586675070, 164.8889363646316610, 310.1175901861107036 ) ) ;
#10492 = CARTESIAN_POINT ( 'NONE',  ( -106.1636641531658398, 79.04398536104955042, 28.79715981783285628 ) ) ;
#10493 = PLANE ( 'NONE',  #2687 ) ;
#10494 = CARTESIAN_POINT ( 'NONE',  ( -9.065023647928146744, 109.7167603697149474, 130.3064260814875013 ) ) ;
#10495 = VECTOR ( 'NONE', #17025, 1000.000000000000114 ) ;
#10496 = CARTESIAN_POINT ( 'NONE',  ( 104.8202145123290876, 69.99999999999998579, -33.35749735200946731 ) ) ;
#10497 = EDGE_CURVE ( 'NONE', #22554, #17125, #13118, .T. ) ;
#10498 = ORIENTED_EDGE ( 'NONE', *, *, #1773, .F. ) ;
#10499 = ADVANCED_FACE ( 'NONE', ( #6205 ), #22028, .F. ) ;
#10500 = CARTESIAN_POINT ( 'NONE',  ( -16.77414143088337184, 138.3748544051812246, 249.7078392314084567 ) ) ;
#10501 = ADVANCED_FACE ( 'NONE', ( #11846 ), #6332, .F. ) ;
#10502 = ORIENTED_EDGE ( 'NONE', *, *, #656, .T. ) ;
#10503 = ORIENTED_EDGE ( 'NONE', *, *, #3503, .F. ) ;
#10504 = VERTEX_POINT ( 'NONE', #10115 ) ;
#10505 = ADVANCED_FACE ( 'NONE', ( #2868 ), #9879, .F. ) ;
#10506 = CARTESIAN_POINT ( 'NONE',  ( 18.55084795937754905, 185.3714166030938770, 310.7056270676168310 ) ) ;
#10507 = ORIENTED_EDGE ( 'NONE', *, *, #14030, .T. ) ;
#10508 = PLANE ( 'NONE',  #12426 ) ;
#10509 = DIRECTION ( 'NONE',  ( -0.9999164797902015955, -6.965998958219364448E-18, 0.01292414190464157182 ) ) ;
#10510 = CARTESIAN_POINT ( 'NONE',  ( 164.0000000000000000, 20.00000000000000000, -2.290411758281096087E-12 ) ) ;
#10511 = CARTESIAN_POINT ( 'NONE',  ( 64.10672825728823909, 104.3814432989690602, -69.53080186952975339 ) ) ;
#10512 = EDGE_CURVE ( 'NONE', #8095, #3063, #7127, .T. ) ;
#10513 = CARTESIAN_POINT ( 'NONE',  ( 0.000000000000000000, 1.999999999999998224, 0.000000000000000000 ) ) ;
#10514 = LINE ( 'NONE', #10400, #21395 ) ;
#10515 = CARTESIAN_POINT ( 'NONE',  ( 12.08126718300561109, 187.6900170120506459, 307.7358539476931583 ) ) ;
#10516 = CARTESIAN_POINT ( 'NONE',  ( 90.14522075562641135, 79.46791348803257904, 27.62924625256333044 ) ) ;
#10517 = CARTESIAN_POINT ( 'NONE',  ( -110.8973471360828285, 103.0000000000000000, -68.71519772349600430 ) ) ;
#10518 =( NAMED_UNIT ( * ) SI_UNIT ( $, .STERADIAN. ) SOLID_ANGLE_UNIT ( ) );
#10519 = CARTESIAN_POINT ( 'NONE',  ( 91.62437796271727564, 95.44063823554748183, 60.86849236629024773 ) ) ;
#10520 = EDGE_CURVE ( 'NONE', #22544, #14939, #4682, .T. ) ;
#10521 = CARTESIAN_POINT ( 'NONE',  ( 51.50086788761742440, 181.5071008296286266, 255.8949677505804061 ) ) ;
#10522 = DIRECTION ( 'NONE',  ( 0.9909299940865187173, -0.1338359446631179062, -0.01207007604876208194 ) ) ;
#10523 = VERTEX_POINT ( 'NONE', #1289 ) ;
#10524 = CARTESIAN_POINT ( 'NONE',  ( -92.55117574443677597, 77.19412514573775752, -28.91372802644275453 ) ) ;
#10525 = ORIENTED_EDGE ( 'NONE', *, *, #21536, .F. ) ;
#10526 = CARTESIAN_POINT ( 'NONE',  ( 10.99126027451603171, 140.4227465520236535, 76.62731417366427422 ) ) ;
#10527 = CARTESIAN_POINT ( 'NONE',  ( 3.072605476372664679, 191.4131571344979932, 256.4662960534838589 ) ) ;
#10528 = CARTESIAN_POINT ( 'NONE',  ( 1.364374644014609697E-14, 69.99999999999998579, -9.836443712999143722E-15 ) ) ;
#10529 = EDGE_CURVE ( 'NONE', #12252, #11456, #8272, .T. ) ;
#10530 = ORIENTED_EDGE ( 'NONE', *, *, #16282, .T. ) ;
#10531 = CARTESIAN_POINT ( 'NONE',  ( 13.04191424503058450, 190.3037527154888551, 320.8502931330203296 ) ) ;
#10532 = EDGE_LOOP ( 'NONE', ( #11008, #8956, #7646, #9929 ) ) ;
#10533 = ORIENTED_EDGE ( 'NONE', *, *, #219, .T. ) ;
#10534 = FACE_OUTER_BOUND ( 'NONE', #11071, .T. ) ;
#10535 = VECTOR ( 'NONE', #1322, 1000.000000000000227 ) ;
#10536 = CARTESIAN_POINT ( 'NONE',  ( 52.02138963284384943, 106.9476250623077789, 70.12004797256865629 ) ) ;
#10537 = CARTESIAN_POINT ( 'NONE',  ( -8.992099355616254286, 184.9255222043797176, 323.2302142135638974 ) ) ;
#10538 = CARTESIAN_POINT ( 'NONE',  ( 9.028305489318197985, 166.3693967048470199, 83.51031826593310825 ) ) ;
#10539 = PLANE ( 'NONE',  #18397 ) ;
#10540 = ORIENTED_EDGE ( 'NONE', *, *, #58, .T. ) ;
#10541 = CARTESIAN_POINT ( 'NONE',  ( -49.99582398951009310, 170.0000000000008242, 0.6462070952329234119 ) ) ;
#10542 = CARTESIAN_POINT ( 'NONE',  ( -90.50186546057693704, 78.02565673216736286, 32.58161589089091592 ) ) ;
#10543 = CYLINDRICAL_SURFACE ( 'NONE', #11733, 3.399999999999985700 ) ;
#10544 = CARTESIAN_POINT ( 'NONE',  ( -14.68167319698930129, 180.7010392265696908, 317.4437403699121205 ) ) ;
#10545 = ORIENTED_EDGE ( 'NONE', *, *, #12481, .F. ) ;
#10546 = CARTESIAN_POINT ( 'NONE',  ( 19.14166374449356312, 175.4877217292663545, 88.21204820665161606 ) ) ;
#10547 = DIRECTION ( 'NONE',  ( 0.9770372205688160339, -0.2127605332646582970, -0.01145535281434409587 ) ) ;
#10548 = DIRECTION ( 'NONE',  ( -0.01292394549866632963, -0.005513023399716958026, -0.9999012842304692006 ) ) ;
#10549 = DIRECTION ( 'NONE',  ( -2.449293598294706414E-16, -0.000000000000000000, -1.000000000000000000 ) ) ;
#10550 = AXIS2_PLACEMENT_3D ( 'NONE', #6100, #4024, #9323 ) ;
#10551 = LINE ( 'NONE', #15860, #14792 ) ;
#10552 = CONTEXT_DEPENDENT_SHAPE_REPRESENTATION ( #3675, #15639 ) ;
#10553 = DIRECTION ( 'NONE',  ( 0.9999164797902015955, 6.965998958219364448E-18, -0.01292414190464157182 ) ) ;
#10554 = CARTESIAN_POINT ( 'NONE',  ( -48.73516844915841517, 109.8600507193323921, -43.54289476181637042 ) ) ;
#10555 = CARTESIAN_POINT ( 'NONE',  ( 4.855148840260169685, 158.0578537176658926, 299.6314082057050427 ) ) ;
#10556 = EDGE_CURVE ( 'NONE', #99, #5930, #19280, .T. ) ;
#10557 = CYLINDRICAL_SURFACE ( 'NONE', #20187, 95.00000000000001421 ) ;
#10558 = ADVANCED_FACE ( 'NONE', ( #18938 ), #9386, .F. ) ;
#10559 = CARTESIAN_POINT ( 'NONE',  ( 92.40872671617952960, 72.00000000000000000, -33.19707612406970298 ) ) ;
#10560 = EDGE_LOOP ( 'NONE', ( #19740, #15680, #7382, #16065 ) ) ;
#10561 = ORIENTED_EDGE ( 'NONE', *, *, #3162, .T. ) ;
#10562 = CARTESIAN_POINT ( 'NONE',  ( 158.3970384574715524, 1.999999999999998224, -62.74304228515679682 ) ) ;
#10563 = CARTESIAN_POINT ( 'NONE',  ( -56.11438623100815448, 126.5883500096207683, 107.5739081604535414 ) ) ;
#10564 = ORIENTED_EDGE ( 'NONE', *, *, #7116, .F. ) ;
#10565 = CARTESIAN_POINT ( 'NONE',  ( 51.53948562937888767, 109.2346207935383120, -44.83551851856461923 ) ) ;
#10566 = ORIENTED_EDGE ( 'NONE', *, *, #10085, .F. ) ;
#10567 =( NAMED_UNIT ( * ) PLANE_ANGLE_UNIT ( ) SI_UNIT ( $, .RADIAN. ) );
#10568 = DIRECTION ( 'NONE',  ( 0.009760756503427813965, -0.9999378516499565217, 0.005387065077607405654 ) ) ;
#10569 = DIRECTION ( 'NONE',  ( 7.125109674403838460E-05, -0.9999848031710254492, 0.005512562950847868688 ) ) ;
#10570 = DIRECTION ( 'NONE',  ( 0.01292414190464131508, 1.902755938799530474E-22, 0.9999164797902017066 ) ) ;
#10571 = CIRCLE ( 'NONE', #6882, 95.00000000000004263 ) ;
#10572 = CARTESIAN_POINT ( 'NONE',  ( -4.433483160726415129, 326.8290646393697898, 320.1652560256880520 ) ) ;
#10573 = EDGE_LOOP ( 'NONE', ( #16649, #1610 ) ) ;
#10574 = AXIS2_PLACEMENT_3D ( 'NONE', #12911, #7606, #2332 ) ;
#10575 = CARTESIAN_POINT ( 'NONE',  ( -45.67488410632294915, 171.6105373975396162, -51.92370490599741117 ) ) ;
#10576 = CARTESIAN_POINT ( 'NONE',  ( -88.16661084868957232, 88.54544711483490005, 52.63461214281247891 ) ) ;
#10577 = VERTEX_POINT ( 'NONE', #17353 ) ;
#10578 = COLOUR_RGB ( '', 0.40784314, 0.44705882, 0.49803922) ;
#10579 = ORIENTED_EDGE ( 'NONE', *, *, #6954, .F. ) ;
#10580 = DIRECTION ( 'NONE',  ( 0.1337561903331557223, 0.9909881666746205298, -0.007192708699472579598 ) ) ;
#10581 = LINE ( 'NONE', #19077, #6312 ) ;
#10582 = EDGE_CURVE ( 'NONE', #1810, #14816, #12344, .T. ) ;
#10583 = CARTESIAN_POINT ( 'NONE',  ( 80.26441115539796556, 75.13699351169600504, -6.137861275126254235 ) ) ;
#10584 = CARTESIAN_POINT ( 'NONE',  ( -55.33894950108811628, 126.9191314136040063, 167.5679852142817197 ) ) ;
#10585 = ORIENTED_EDGE ( 'NONE', *, *, #9406, .T. ) ;
#10586 = DIRECTION ( 'NONE',  ( -1.000000000000000000, 0.000000000000000000, 0.000000000000000000 ) ) ;
#10587 = ORIENTED_EDGE ( 'NONE', *, *, #13962, .T. ) ;
#10588 = CARTESIAN_POINT ( 'NONE',  ( 65.34111304903984774, 145.1470193978928478, 25.89384641848939239 ) ) ;
#10589 = CARTESIAN_POINT ( 'NONE',  ( -76.67152933958324468, 75.07738311394996344, -2.850188674051770121 ) ) ;
#10590 = FACE_OUTER_BOUND ( 'NONE', #14025, .T. ) ;
#10591 = AXIS2_PLACEMENT_3D ( 'NONE', #14652, #739, #861 ) ;
#10592 = EDGE_LOOP ( 'NONE', ( #2217, #6290, #17739, #9438 ) ) ;
#10593 = CARTESIAN_POINT ( 'NONE',  ( 8.957006556259601737, 157.7978957687922446, 81.55830191989343803 ) ) ;
#10594 = DIRECTION ( 'NONE',  ( -0.01292394549866741384, -0.005513023399720269613, -0.9999012842304692006 ) ) ;
#10595 = CARTESIAN_POINT ( 'NONE',  ( 1.121675378414705104, 55.00000000000000000, 109.9942809619911799 ) ) ;
#10596 = CIRCLE ( 'NONE', #699, 2.000000000000000000 ) ;
#10597 = CARTESIAN_POINT ( 'NONE',  ( -51.06998696435687179, 114.2155732021687840, 164.9875346684564192 ) ) ;
#10598 = ORIENTED_EDGE ( 'NONE', *, *, #21123, .T. ) ;
#10599 = EDGE_CURVE ( 'NONE', #14514, #17969, #4239, .T. ) ;
#10600 = DIRECTION ( 'NONE',  ( 0.000000000000000000, 1.000000000000000000, -0.000000000000000000 ) ) ;
#10601 = VERTEX_POINT ( 'NONE', #5903 ) ;
#10602 = VERTEX_POINT ( 'NONE', #17703 ) ;
#10603 = CARTESIAN_POINT ( 'NONE',  ( 19.94311012550880946, 183.4975381809269095, 314.2664455249164348 ) ) ;
#10604 = EDGE_CURVE ( 'NONE', #8847, #10113, #11974, .T. ) ;
#10605 = AXIS2_PLACEMENT_3D ( 'NONE', #4124, #5974, #701 ) ;
#10607 = ORIENTED_EDGE ( 'NONE', *, *, #18084, .F. ) ;
#10606 = ORIENTED_EDGE ( 'NONE', *, *, #19735, .T. ) ;
#10608 = DIRECTION ( 'NONE',  ( -0.3834992599886432596, 0.005063754594578209756, 0.9235273011544211652 ) ) ;
#10609 = CARTESIAN_POINT ( 'NONE',  ( -1.163172771417702700, 69.99999999999998579, -89.99248318111824574 ) ) ;
#10610 = AXIS2_PLACEMENT_3D ( 'NONE', #19850, #3796, #17840 ) ;
#10611 = CARTESIAN_POINT ( 'NONE',  ( -10.97106015414653157, 147.1489019915714209, 278.5469242478091019 ) ) ;
#10612 = ADVANCED_FACE ( 'NONE', ( #116 ), #7921, .T. ) ;
#10613 = DIRECTION ( 'NONE',  ( 0.01292414190464131335, 0.000000000000000000, 0.9999164797902017066 ) ) ;
#10614 = DIRECTION ( 'NONE',  ( -0.8981428216242027807, 0.000000000000000000, 0.4397038457472431938 ) ) ;
#10615 = EDGE_CURVE ( 'NONE', #12915, #4144, #6315, .T. ) ;
#10616 = CARTESIAN_POINT ( 'NONE',  ( 81.33532363055485348, 75.19538212720385673, -7.141617114204432681 ) ) ;
#10617 = CARTESIAN_POINT ( 'NONE',  ( 14.01676522198601660, 186.8106453161406648, 305.2787119402084386 ) ) ;
#10618 = DIRECTION ( 'NONE',  ( -0.01297756288283796570, 0.000000000000000000, -0.9999157878849708192 ) ) ;
#10619 = DIRECTION ( 'NONE',  ( -0.01292414190463827932, 0.000000000000000000, -0.9999164797902018176 ) ) ;
#10620 = STYLED_ITEM ( 'NONE', ( #3718 ), #17529 ) ;
#10621 = EDGE_CURVE ( 'NONE', #22622, #22296, #8698, .T. ) ;
#10622 = CARTESIAN_POINT ( 'NONE',  ( 90.82246629754764911, 169.9999999999999716, -1.173900486973972868 ) ) ;
#10623 = DIRECTION ( 'NONE',  ( 0.7944560844389294552, 0.000000000000000000, 0.6073216033519345247 ) ) ;
#10624 = AXIS2_PLACEMENT_3D ( 'NONE', #19943, #16425, #9273 ) ;
#10625 = EDGE_LOOP ( 'NONE', ( #21570, #22473, #8897 ) ) ;
#10626 = CARTESIAN_POINT ( 'NONE',  ( -92.88576702167225108, 79.82922271357917055, -28.81576165492124986 ) ) ;
#10627 = VERTEX_POINT ( 'NONE', #14020 ) ;
#10628 = ORIENTED_EDGE ( 'NONE', *, *, #8992, .F. ) ;
#10629 = ADVANCED_FACE ( 'NONE', ( #19166 ), #9011, .T. ) ;
#10630 = CARTESIAN_POINT ( 'NONE',  ( -68.97076059960821226, 70.03291683438813209, -85.69217454375159093 ) ) ;
#10631 = DIRECTION ( 'NONE',  ( 0.3101392564284315978, 0.9506461370142478273, -0.009250070373107145000 ) ) ;
#10632 = PRODUCT_DEFINITION_CONTEXT ( 'detailed design', #2661, 'design' ) ;
#10633 = VECTOR ( 'NONE', #4592, 1000.000000000000000 ) ;
#10634 = EDGE_LOOP ( 'NONE', ( #7291, #15880, #20127, #8 ) ) ;
#10635 = CARTESIAN_POINT ( 'NONE',  ( -7.798485590386990296, 70.56130593988649480, -82.51270763647208639 ) ) ;
#10636 = VECTOR ( 'NONE', #13267, 1000.000000000000114 ) ;
#10637 = CARTESIAN_POINT ( 'NONE',  ( 42.84128820176451313, 101.1708071963161615, 64.81746289747974288 ) ) ;
#10638 = ADVANCED_FACE ( 'NONE', ( #22359 ), #10867, .F. ) ;
#10639 = VERTEX_POINT ( 'NONE', #12183 ) ;
#10640 = DIRECTION ( 'NONE',  ( 0.9909299940865187173, -0.1338359446631173233, -0.01207007604876291287 ) ) ;
#10641 = CARTESIAN_POINT ( 'NONE',  ( -54.06627702000321989, 114.3880670778429476, 162.4281343095261718 ) ) ;
#10642 = DIRECTION ( 'NONE',  ( 7.125109674364534776E-05, -0.9999848031710252272, 0.005512562950849704893 ) ) ;
#10643 = DIRECTION ( 'NONE',  ( -7.125109674118361251E-05, 0.9999848031710253382, -0.005512562950849477644 ) ) ;
#10644 = CARTESIAN_POINT ( 'NONE',  ( -8.753245784830484766, 185.8505709766340317, 321.2394042940741770 ) ) ;
#10645 = AXIS2_PLACEMENT_3D ( 'NONE', #18817, #17109, #3420 ) ;
#10647 = CARTESIAN_POINT ( 'NONE',  ( -164.0000000000000000, 20.00000000000000000, 8.000000000000019540 ) ) ;
#10646 = CARTESIAN_POINT ( 'NONE',  ( 146.5000000000000000, 18.00000000000000355, -2.025191382850354537E-12 ) ) ;
#10648 = DIRECTION ( 'NONE',  ( 5.440186201345738641E-18, 1.000000000000000000, 1.334940939666364181E-17 ) ) ;
#10649 = ORIENTED_EDGE ( 'NONE', *, *, #22012, .F. ) ;
#10650 = CARTESIAN_POINT ( 'NONE',  ( -14.11939326714681364, 181.9331570759241856, 318.5758607607144199 ) ) ;
#10651 = EDGE_LOOP ( 'NONE', ( #13928, #14563, #21119, #2784 ) ) ;
#10652 = CYLINDRICAL_SURFACE ( 'NONE', #4758, 95.00000000000001421 ) ;
#10653 = DIRECTION ( 'NONE',  ( 0.7069973413461614342, 0.7070960354057256314, -0.01303671902605248872 ) ) ;
#10654 = CARTESIAN_POINT ( 'NONE',  ( -15.54784124399456502, 177.7690436490937316, 314.1134455231556331 ) ) ;
#10655 = VECTOR ( 'NONE', #3942, 1000.000000000000000 ) ;
#10656 = ORIENTED_EDGE ( 'NONE', *, *, #10354, .F. ) ;
#10657 = VECTOR ( 'NONE', #723, 1000.000000000000114 ) ;
#10658 = CARTESIAN_POINT ( 'NONE',  ( 15.77808660118132700, 185.8345873904136170, 306.0719219466911909 ) ) ;
#10659 = EDGE_CURVE ( 'NONE', #18024, #9297, #6656, .T. ) ;
#10660 = VECTOR ( 'NONE', #5481, 1000.000000000000114 ) ;
#10661 = CARTESIAN_POINT ( 'NONE',  ( -40.33104288128404846, 94.48610424851698042, 83.91830964824988826 ) ) ;
#10662 = AXIS2_PLACEMENT_3D ( 'NONE', #995, #7982, #4301 ) ;
#10663 = EDGE_LOOP ( 'NONE', ( #11026, #4345, #8401, #3656 ) ) ;
#10664 = DIRECTION ( 'NONE',  ( -5.440186201345738641E-18, -1.000000000000000000, -1.334940939666364181E-17 ) ) ;
#10665 = VECTOR ( 'NONE', #14211, 999.9999999999998863 ) ;
#10666 = DIRECTION ( 'NONE',  ( -0.6933298757296632031, -0.07639711794142747814, 0.7165592535100873128 ) ) ;
#10667 = EDGE_CURVE ( 'NONE', #16597, #19220, #14261, .T. ) ;
#10668 = DIRECTION ( 'NONE',  ( 7.125109674364536131E-05, -0.9999848031710253382, 0.005512562950849705760 ) ) ;
#10669 = CARTESIAN_POINT ( 'NONE',  ( -10.89768303757167800, 114.0778156631497353, 123.2533725142381229 ) ) ;
#10670 = VECTOR ( 'NONE', #12445, 1000.000000000000000 ) ;
#10671 = ORIENTED_EDGE ( 'NONE', *, *, #6348, .F. ) ;
#10672 = DIRECTION ( 'NONE',  ( 0.000000000000000000, 0.000000000000000000, 1.000000000000000000 ) ) ;
#10673 = DIRECTION ( 'NONE',  ( 0.000000000000000000, 0.000000000000000000, 1.000000000000000000 ) ) ;
#10674 = CARTESIAN_POINT ( 'NONE',  ( 3.872354045398203937, 166.6517708494369856, 299.5967279023338392 ) ) ;
#10675 = CONICAL_SURFACE ( 'NONE', #20564, 5.000000000000023981, 0.7853981633974460586 ) ;
#10676 = EDGE_LOOP ( 'NONE', ( #8022, #3023, #19941, #18989 ) ) ;
#10677 = DIRECTION ( 'NONE',  ( -0.9999164797902017066, 1.387778780781447253E-14, 0.01292414190463832269 ) ) ;
#10678 = ORIENTED_EDGE ( 'NONE', *, *, #1241, .T. ) ;
#10679 = CARTESIAN_POINT ( 'NONE',  ( -41.94137166082473556, 162.5796238295972671, 273.2086669205137355 ) ) ;
#10680 = FACE_OUTER_BOUND ( 'NONE', #21848, .T. ) ;
#10681 = CARTESIAN_POINT ( 'NONE',  ( -50.56780451594417514, 125.7553391191873544, -43.60684728318641845 ) ) ;
#10682 = ORIENTED_EDGE ( 'NONE', *, *, #17625, .T. ) ;
#10683 = ORIENTED_EDGE ( 'NONE', *, *, #6427, .T. ) ;
#10684 = DIRECTION ( 'NONE',  ( 0.000000000000000000, 1.000000000000000000, -0.000000000000000000 ) ) ;
#10685 = CARTESIAN_POINT ( 'NONE',  ( -20.57130763759250414, 139.7551263635816952, -44.07174742163757486 ) ) ;
#10686 = AXIS2_PLACEMENT_3D ( 'NONE', #4179, #18311, #633 ) ;
#10687 = DIRECTION ( 'NONE',  ( 7.125109674403837105E-05, -0.9999848031710252272, 0.005512562950847867821 ) ) ;
#10688 = EDGE_CURVE ( 'NONE', #1991, #3937, #12304, .T. ) ;
#10689 = EDGE_CURVE ( 'NONE', #4095, #11132, #18919, .T. ) ;
#10690 = ORIENTED_EDGE ( 'NONE', *, *, #17310, .F. ) ;
#10691 = CARTESIAN_POINT ( 'NONE',  ( 50.34170926724522843, 140.1470898690143372, 26.11428438467088142 ) ) ;
#10692 = AXIS2_PLACEMENT_3D ( 'NONE', #6812, #19097, #22517 ) ;
#10693 = CARTESIAN_POINT ( 'NONE',  ( -88.16755730635141219, 88.61500917853037151, 52.54598585929731058 ) ) ;
#10694 =( GEOMETRIC_REPRESENTATION_CONTEXT ( 3 ) GLOBAL_UNCERTAINTY_ASSIGNED_CONTEXT ( ( #1027 ) ) GLOBAL_UNIT_ASSIGNED_CONTEXT ( ( #12937, #11310, #7522 ) ) REPRESENTATION_CONTEXT ( 'NONE', 'WORKASPACE' ) );
#10695 = VECTOR ( 'NONE', #6697, 999.9999999999998863 ) ;
#10696 = ORIENTED_EDGE ( 'NONE', *, *, #2370, .T. ) ;
#10697 = VERTEX_POINT ( 'NONE', #8477 ) ;
#10698 = DIRECTION ( 'NONE',  ( 0.9506032891036977350, -0.3102281881984299550, -0.01057629388543066158 ) ) ;
#10699 = AXIS2_PLACEMENT_3D ( 'NONE', #4782, #5121, #13992 ) ;
#10700 = DIRECTION ( 'NONE',  ( -0.3102455404053335308, -0.9506564598521395348, 0.000000000000000000 ) ) ;
#10701 = EDGE_LOOP ( 'NONE', ( #12567, #574, #12509, #14629, #5852, #8380 ) ) ;
#10702 = CARTESIAN_POINT ( 'NONE',  ( 81.69827340936640780, 75.12327740397421394, 3.784263597974759641 ) ) ;
#10703 = CARTESIAN_POINT ( 'NONE',  ( -55.33804461215960657, 114.2193244133317904, 167.6379947637574617 ) ) ;
#10704 = DIRECTION ( 'NONE',  ( -5.440186201345738641E-18, -1.000000000000000000, -1.334940939666364181E-17 ) ) ;
#10705 = VERTEX_POINT ( 'NONE', #3546 ) ;
#10706 = DIRECTION ( 'NONE',  ( 0.009760756503428015193, -0.9999378516499566327, 0.005387065077612487526 ) ) ;
#10707 = VERTEX_POINT ( 'NONE', #10562 ) ;
#10708 = CARTESIAN_POINT ( 'NONE',  ( -162.0000000000000000, 20.00000000000000000, 10.00000000000001954 ) ) ;
#10709 = CARTESIAN_POINT ( 'NONE',  ( 1.364374644014609697E-14, 69.99999999999998579, -9.836443712999143722E-15 ) ) ;
#10710 = CYLINDRICAL_SURFACE ( 'NONE', #14971, 2.000000000000001332 ) ;
#10711 = CARTESIAN_POINT ( 'NONE',  ( -22.45062868030126779, 324.7702718825011630, 320.5707452954474661 ) ) ;
#10712 = CIRCLE ( 'NONE', #16609, 4.200000000000005507 ) ;
#10713 = VECTOR ( 'NONE', #4563, 999.9999999999998863 ) ;
#10714 = VERTEX_POINT ( 'NONE', #15524 ) ;
#10715 = CARTESIAN_POINT ( 'NONE',  ( -105.5195728421876282, 78.18109283220577765, 31.07451122637823815 ) ) ;
#10716 = DIRECTION ( 'NONE',  ( 0.01292394549866734098, 0.005513023399720419666, 0.9999012842304692006 ) ) ;
#10717 = CARTESIAN_POINT ( 'NONE',  ( -29.40402206585522293, 189.4003865961453812, -108.4455932242574789 ) ) ;
#10718 = CIRCLE ( 'NONE', #18777, 95.00000000000001421 ) ;
#10719 = CARTESIAN_POINT ( 'NONE',  ( 395.1215762121263992, 103.0000000000000000, -76.28455149755049547 ) ) ;
#10720 = ORIENTED_EDGE ( 'NONE', *, *, #19390, .F. ) ;
#10721 = AXIS2_PLACEMENT_3D ( 'NONE', #1527, #11980, #17258 ) ;
#10722 = CARTESIAN_POINT ( 'NONE',  ( -72.51438462527775641, 87.23323244114081376, 69.92599951943640235 ) ) ;
#10723 = EDGE_LOOP ( 'NONE', ( #9465, #7258 ) ) ;
#10724 = ORIENTED_EDGE ( 'NONE', *, *, #7950, .F. ) ;
#10725 = ORIENTED_EDGE ( 'NONE', *, *, #8937, .F. ) ;
#10726 = CARTESIAN_POINT ( 'NONE',  ( 18.22858106979587234, 185.9398809517860514, 318.3817688168216478 ) ) ;
#10727 = CIRCLE ( 'NONE', #5943, 110.5324305509042233 ) ;
#10729 = ORIENTED_EDGE ( 'NONE', *, *, #1938, .F. ) ;
#10728 = EDGE_LOOP ( 'NONE', ( #14108, #20818, #22662, #7079 ) ) ;
#10730 = VECTOR ( 'NONE', #5601, 999.9999999999998863 ) ;
#10731 = AXIS2_PLACEMENT_3D ( 'NONE', #10977, #18745, #16403 ) ;
#10732 = CARTESIAN_POINT ( 'NONE',  ( 157.5176307659771169, 18.00000000000000355, 60.94675664190834397 ) ) ;
#10733 = CARTESIAN_POINT ( 'NONE',  ( 41.14495236153211977, 95.00650438983588231, -44.60766223544680287 ) ) ;
#10734 = CARTESIAN_POINT ( 'NONE',  ( -8.648597540386568028, 145.5673199092568950, 277.8375784336965353 ) ) ;
#10735 = CARTESIAN_POINT ( 'NONE',  ( 0.000000000000000000, 45.00000000000000711, 0.000000000000000000 ) ) ;
#10736 = EDGE_CURVE ( 'NONE', #22518, #2811, #972, .T. ) ;
#10737 = CARTESIAN_POINT ( 'NONE',  ( -65.67450334697799974, 189.7102623349352086, -51.76499945731497121 ) ) ;
#10738 = CARTESIAN_POINT ( 'NONE',  ( -55.33804461215960657, 114.2193244133317904, 167.6379947637574617 ) ) ;
#10739 = CARTESIAN_POINT ( 'NONE',  ( 13.04683326300609636, 190.3009515221012862, 320.8498797597175667 ) ) ;
#10740 = CARTESIAN_POINT ( 'NONE',  ( -14.53239793090661180, 175.6255473142593644, 113.6490011371711688 ) ) ;
#10741 = CARTESIAN_POINT ( 'NONE',  ( 17.45373000089112381, 184.7724903878686291, 309.3158825916956971 ) ) ;
#10742 = CARTESIAN_POINT ( 'NONE',  ( 92.88576702167598853, 79.82922271357915633, 28.81576165492026931 ) ) ;
#10743 = DIRECTION ( 'NONE',  ( -0.01292394549866750231, -0.005513023399722823126, -0.9999012842304692006 ) ) ;
#10744 = B_SPLINE_CURVE_WITH_KNOTS ( 'NONE', 3,
 ( #6370, #17394, #13391, #22405 ),
 .UNSPECIFIED., .F., .F.,
 ( 4, 4 ),
 ( 0.03593651043649991050, 0.03600679027956682487 ),
 .UNSPECIFIED. ) ;
#10745 = CARTESIAN_POINT ( 'NONE',  ( 58.87600894486503478, 126.5883500096209815, 106.0876318414197499 ) ) ;
#10746 = AXIS2_PLACEMENT_3D ( 'NONE', #20171, #2506, #5946 ) ;
#10747 = ADVANCED_FACE ( 'NONE', ( #17582 ), #15869, .F. ) ;
#10748 = VECTOR ( 'NONE', #22041, 1000.000000000000000 ) ;
#10749 = CARTESIAN_POINT ( 'NONE',  ( -14.02864438394164459, 325.7329298795127670, 320.4531201330283352 ) ) ;
#10750 = FACE_OUTER_BOUND ( 'NONE', #2435, .T. ) ;
#10751 = VERTEX_POINT ( 'NONE', #4198 ) ;
#10752 = CARTESIAN_POINT ( 'NONE',  ( -91.47552206421207188, 77.76803451549854174, -29.83954006679693549 ) ) ;
#10753 = EDGE_CURVE ( 'NONE', #17793, #650, #7938, .T. ) ;
#10754 = ORIENTED_EDGE ( 'NONE', *, *, #5439, .F. ) ;
#10755 = EDGE_CURVE ( 'NONE', #22032, #20005, #20014, .T. ) ;
#10756 = CARTESIAN_POINT ( 'NONE',  ( -5.156377330703347361, 81.19615242270661781, -99.58697729741749072 ) ) ;
#10757 = CYLINDRICAL_SURFACE ( 'NONE', #2870, 7.499999999999991118 ) ;
#10758 = AXIS2_PLACEMENT_3D ( 'NONE', #5920, #4076, #14679 ) ;
#10759 = CIRCLE ( 'NONE', #5981, 3.399999999999985700 ) ;
#10760 = CARTESIAN_POINT ( 'NONE',  ( -64.54884397553028919, 190.1904397277864973, 35.32514273129017113 ) ) ;
#10761 = EDGE_CURVE ( 'NONE', #2857, #15210, #18350, .T. ) ;
#10762 = CARTESIAN_POINT ( 'NONE',  ( -44.65237404513518271, 168.6466622724118452, 27.18596972279685531 ) ) ;
#10763 = EDGE_LOOP ( 'NONE', ( #20452, #4775 ) ) ;
#10764 = DIRECTION ( 'NONE',  ( 7.125109674161246868E-05, -0.9999848031710253382, 0.005512562950850155054 ) ) ;
#10765 = ORIENTED_EDGE ( 'NONE', *, *, #8103, .T. ) ;
#10766 = CARTESIAN_POINT ( 'NONE',  ( -54.52327687265813694, 20.00000000000000000, 111.3697098814011781 ) ) ;
#10767 = EDGE_CURVE ( 'NONE', #17449, #7530, #13079, .T. ) ;
#10768 = CARTESIAN_POINT ( 'NONE',  ( 64.99457118636310327, 170.0000000000000284, -0.8400692238017243296 ) ) ;
#10769 = CARTESIAN_POINT ( 'NONE',  ( -11.74988407969402360, 185.7573108837101756, 320.6989643996056998 ) ) ;
#10770 = CARTESIAN_POINT ( 'NONE',  ( -90.67285013207035149, 77.76891457534604513, 32.19520807900870807 ) ) ;
#10771 = DIRECTION ( 'NONE',  ( 0.9999164797902015955, 2.457859219970326020E-15, -0.01292414190464043211 ) ) ;
#10772 = TOROIDAL_SURFACE ( 'NONE', #6384, 21.67179167071591550, 2.000000000000000000 ) ;
#10773 = ORIENTED_EDGE ( 'NONE', *, *, #20746, .T. ) ;
#10774 = CARTESIAN_POINT ( 'NONE',  ( -13.52516265657463812, 183.2462493215299162, 309.9645816984750013 ) ) ;
#10775 = ORIENTED_EDGE ( 'NONE', *, *, #4008, .T. ) ;
#10776 = DIRECTION ( 'NONE',  ( -0.9999164797902015955, -4.476705744456278510E-15, 0.01292414190464144692 ) ) ;
#10777 = DIRECTION ( 'NONE',  ( 0.01035335185279153900, 0.005513005182355262476, 0.9999312050732647172 ) ) ;
#10778 = CARTESIAN_POINT ( 'NONE',  ( -15.16713580098303638, 179.5535043013633754, 314.1163235527705524 ) ) ;
#10779 = AXIS2_PLACEMENT_3D ( 'NONE', #4619, #16938, #3015 ) ;
#10780 = ADVANCED_FACE ( 'NONE', ( #2483 ), #12643, .F. ) ;
#10781 = AXIS2_PLACEMENT_3D ( 'NONE', #16042, #17636, #5548 ) ;
#10782 = CARTESIAN_POINT ( 'NONE',  ( 20.38555108690226447, 182.1783941675930691, 312.0429188998837162 ) ) ;
#10783 = EDGE_CURVE ( 'NONE', #5077, #11631, #12239, .T. ) ;
#10784 = EDGE_CURVE ( 'NONE', #9371, #4637, #11465, .T. ) ;
#10785 = VERTEX_POINT ( 'NONE', #14922 ) ;
#10786 = EDGE_CURVE ( 'NONE', #5976, #17630, #2329, .T. ) ;
#10787 = DIRECTION ( 'NONE',  ( -0.9999164797902015955, -2.001050586450178695E-22, 0.01292414190464131335 ) ) ;
#10788 = FACE_OUTER_BOUND ( 'NONE', #1293, .T. ) ;
#10789 = VECTOR ( 'NONE', #10378, 999.9999999999998863 ) ;
#10790 = CIRCLE ( 'NONE', #21758, 2.499999999999988010 ) ;
#10791 = VERTEX_POINT ( 'NONE', #2058 ) ;
#10792 = CARTESIAN_POINT ( 'NONE',  ( 51.78636885665599721, 152.2590373701827957, 256.0525387646090394 ) ) ;
#10793 = LINE ( 'NONE', #8816, #13974 ) ;
#10794 = DIRECTION ( 'NONE',  ( 0.9770372205688159228, -0.2127605332646582692, -0.01145535281434409414 ) ) ;
#10795 = ORIENTED_EDGE ( 'NONE', *, *, #1383, .F. ) ;
#10796 = ADVANCED_FACE ( 'NONE', ( #20044 ), #10772, .T. ) ;
#10797 = CIRCLE ( 'NONE', #19940, 6.499999999999998224 ) ;
#10798 = EDGE_LOOP ( 'NONE', ( #15151, #16662, #4755 ) ) ;
#10799 = CARTESIAN_POINT ( 'NONE',  ( 37.51181209962140883, 93.56461422141670425, -83.92720337889311111 ) ) ;
#10800 = CIRCLE ( 'NONE', #21066, 3.399999999999986144 ) ;
#10801 = CARTESIAN_POINT ( 'NONE',  ( -49.26241605170081073, 111.2512799097718386, -43.54375060610340853 ) ) ;
#10802 = VERTEX_POINT ( 'NONE', #21225 ) ;
#10803 = EDGE_CURVE ( 'NONE', #15344, #3120, #15944, .T. ) ;
#10804 = CARTESIAN_POINT ( 'NONE',  ( -50.58840307354613941, 96.06212804229784297, -45.20051882889240602 ) ) ;
#10805 = ORIENTED_EDGE ( 'NONE', *, *, #8893, .F. ) ;
#10806 = ORIENTED_EDGE ( 'NONE', *, *, #14009, .F. ) ;
#10807 = DIRECTION ( 'NONE',  ( -2.459148776293844314E-24, 1.000000000000000000, -1.902597020224326827E-22 ) ) ;
#10808 = CARTESIAN_POINT ( 'NONE',  ( -162.0000000000000000, 18.00000000000000355, 0.000000000000000000 ) ) ;
#10809 = LINE ( 'NONE', #5616, #7623 ) ;
#10810 = DIRECTION ( 'NONE',  ( 0.9999164797902017066, 2.001050586450177285E-22, -0.01292414190464218071 ) ) ;
#10811 = ORIENTED_EDGE ( 'NONE', *, *, #14235, .T. ) ;
#10812 = ORIENTED_EDGE ( 'NONE', *, *, #13167, .F. ) ;
#10813 = CARTESIAN_POINT ( 'NONE',  ( -27.99766143412566421, 170.0000000000008242, 0.3618759733308087312 ) ) ;
#10814 = AXIS2_PLACEMENT_3D ( 'NONE', #2066, #3892, #2411 ) ;
#10815 = CARTESIAN_POINT ( 'NONE',  ( -5.606570624700499827, 326.6956260390930993, 320.3424165449941938 ) ) ;
#10816 = EDGE_CURVE ( 'NONE', #17630, #20863, #996, .T. ) ;
#10817 = CARTESIAN_POINT ( 'NONE',  ( 8.732865712828665750, 190.3249964942741883, 274.4707185275763095 ) ) ;
#10818 = EDGE_LOOP ( 'NONE', ( #427, #9385, #6467, #2963, #16380, #13801, #16482, #8944, #22648, #8661, #9513, #2407, #19706, #15346, #2940, #12020, #2637, #15020, #5590, #11595, #3842, #19788, #5732, #2165 ) ) ;
#10819 = VECTOR ( 'NONE', #17086, 1000.000000000000000 ) ;
#10820 = CONICAL_SURFACE ( 'NONE', #17431, 9.000000000000001776, 1.047197551196594301 ) ;
#10821 = DIRECTION ( 'NONE',  ( 0.01035335185279134471, 0.005513005182356394383, 0.9999312050732649393 ) ) ;
#10822 = CARTESIAN_POINT ( 'NONE',  ( -88.16961949373364860, 88.74519938941557484, 52.34624730313399255 ) ) ;
#10823 = ORIENTED_EDGE ( 'NONE', *, *, #17599, .F. ) ;
#10824 = VERTEX_POINT ( 'NONE', #2602 ) ;
#10825 = DIRECTION ( 'NONE',  ( 7.125109674160258889E-05, -0.9999848031710253382, 0.005512562950849898315 ) ) ;
#10826 = LINE ( 'NONE', #11503, #7910 ) ;
#10827 = DIRECTION ( 'NONE',  ( 0.008205354412248750534, -0.7726059781012502015, 0.6348327927582032570 ) ) ;
#10828 = EDGE_LOOP ( 'NONE', ( #5100, #8214, #17725, #10806 ) ) ;
#10829 = EDGE_CURVE ( 'NONE', #10951, #6274, #13718, .T. ) ;
#10830 = CARTESIAN_POINT ( 'NONE',  ( 91.39645842968023715, 77.87428392844077507, 30.00278187767188243 ) ) ;
#10831 = ORIENTED_EDGE ( 'NONE', *, *, #19326, .T. ) ;
#10832 = CARTESIAN_POINT ( 'NONE',  ( -44.65290842836073182, 176.1465482961945384, 27.14462550066548729 ) ) ;
#10833 = EDGE_CURVE ( 'NONE', #8542, #7339, #15477, .T. ) ;
#10834 = CARTESIAN_POINT ( 'NONE',  ( 53.31522717123864652, 127.4153035195790835, 256.1697555402749913 ) ) ;
#10835 = CARTESIAN_POINT ( 'NONE',  ( -75.98071139535758789, 75.05062594699535339, -2.131736981522680541 ) ) ;
#10836 = CARTESIAN_POINT ( 'NONE',  ( -23.79181689863955285, 324.5651258154593961, 307.7422675453725560 ) ) ;
#10837 = CARTESIAN_POINT ( 'NONE',  ( -105.6376945813395594, 78.65441476617392880, 30.67074184297031536 ) ) ;
#10838 = EDGE_LOOP ( 'NONE', ( #21622, #8118, #21031, #7239, #9399 ) ) ;
#10839 = LINE ( 'NONE', #3482, #5214 ) ;
#10840 = CARTESIAN_POINT ( 'NONE',  ( -40.65822637310711940, 91.17157287525390075, -84.25167897319539634 ) ) ;
#10841 = ORIENTED_EDGE ( 'NONE', *, *, #17934, .F. ) ;
#10842 = LINE ( 'NONE', #17621, #8842 ) ;
#10843 = ORIENTED_EDGE ( 'NONE', *, *, #6740, .F. ) ;
#10844 = PRESENTATION_LAYER_ASSIGNMENT (  '', '', ( #1309 ) ) ;
#10845 = ORIENTED_EDGE ( 'NONE', *, *, #11289, .T. ) ;
#10846 = CARTESIAN_POINT ( 'NONE',  ( -35.08134114990228625, 165.1748757965034144, 269.1052955077829552 ) ) ;
#10847 = CARTESIAN_POINT ( 'NONE',  ( -13.89421726780587996, 325.7902730365928505, 330.8534925327304563 ) ) ;
#10848 = VERTEX_POINT ( 'NONE', #20829 ) ;
#10849 = DIRECTION ( 'NONE',  ( 0.8981428216242066664, 0.000000000000000000, -0.4397038457472354778 ) ) ;
#10850 = CARTESIAN_POINT ( 'NONE',  ( -89.60390812178910380, 70.24399151081296111, 63.08126157891754104 ) ) ;
#10851 = LINE ( 'NONE', #3599, #4341 ) ;
#10852 = DIRECTION ( 'NONE',  ( 0.000000000000000000, 0.000000000000000000, 1.000000000000000000 ) ) ;
#10853 = EDGE_CURVE ( 'NONE', #10072, #17624, #15928, .T. ) ;
#10854 = CARTESIAN_POINT ( 'NONE',  ( 55.40268456415108034, 18.00000000000000355, 113.1659955246503557 ) ) ;
#10855 = EDGE_CURVE ( 'NONE', #1725, #13090, #19186, .T. ) ;
#10856 = CIRCLE ( 'NONE', #18211, 10.00000000000000355 ) ;
#10857 = DIRECTION ( 'NONE',  ( 0.000000000000000000, 1.000000000000000000, -0.000000000000000000 ) ) ;
#10858 = CARTESIAN_POINT ( 'NONE',  ( 20.02494354238641705, 182.5313087350443482, 310.9605567950519003 ) ) ;
#10859 = CARTESIAN_POINT ( 'NONE',  ( 91.28977804672281593, 78.08428866167092508, 30.31923231637453142 ) ) ;
#10860 = DIRECTION ( 'NONE',  ( -0.9934404589540162256, -0.1135548637187056842, 0.01346653032743081423 ) ) ;
#10861 = B_SPLINE_CURVE_WITH_KNOTS ( 'NONE', 3,
 ( #7526, #16052, #290, #7283, #17653, #1902, #9116, #63, #5561, #14324, #408, #12370, #19675, #21295 ),
 .UNSPECIFIED., .F., .F.,
 ( 4, 2, 2, 2, 2, 2, 4 ),
 ( 0.000000000000000000, 0.0009165371227192408397, 0.001374805684078860175, 0.001833074245438479294, 0.002291342806798098413, 0.002749611368157717749, 0.003666148490876996752 ),
 .UNSPECIFIED. ) ;
#10862 = DIRECTION ( 'NONE',  ( -7.125109674025824596E-05, 0.9999848031710253382, -0.005512562950848693549 ) ) ;
#10863 = LINE ( 'NONE', #8766, #18038 ) ;
#10864 = ORIENTED_EDGE ( 'NONE', *, *, #15975, .T. ) ;
#10865 = DIRECTION ( 'NONE',  ( 0.9999164797902015955, 6.965998958219364448E-18, -0.01292414190464157182 ) ) ;
#10866 = ORIENTED_EDGE ( 'NONE', *, *, #10615, .T. ) ;
#10867 = CONICAL_SURFACE ( 'NONE', #14934, 2.499999999999988010, 1.029744258676651425 ) ;
#10868 = DIRECTION ( 'NONE',  ( 7.176269450075762180E-19, -1.000000000000000000, 5.550596000020001457E-17 ) ) ;
#10869 = EDGE_LOOP ( 'NONE', ( #8617, #9694, #11434, #6289 ) ) ;
#10870 = FACE_OUTER_BOUND ( 'NONE', #11743, .T. ) ;
#10871 =( REPRESENTATION_RELATIONSHIP ('NONE','NONE', #11808, #9590 ) REPRESENTATION_RELATIONSHIP_WITH_TRANSFORMATION ( #9872 )SHAPE_REPRESENTATION_RELATIONSHIP( ) );
#10872 = CARTESIAN_POINT ( 'NONE',  ( -41.96503124479402658, 165.8559883853732515, 234.9371320172060678 ) ) ;
#10873 = ORIENTED_EDGE ( 'NONE', *, *, #10333, .F. ) ;
#10874 = CARTESIAN_POINT ( 'NONE',  ( -14.37471740060550118, 109.6998846769365628, 127.3137863664913425 ) ) ;
#10875 = ORIENTED_EDGE ( 'NONE', *, *, #11871, .F. ) ;
#10876 = CARTESIAN_POINT ( 'NONE',  ( -53.58947677482678529, 114.5014335370325824, 162.3651637728053174 ) ) ;
#10877 = ADVANCED_FACE ( 'NONE', ( #6395 ), #20613, .T. ) ;
#10878 = CARTESIAN_POINT ( 'NONE',  ( 70.91392079944857585, 91.32005360614645895, 84.09052168258639881 ) ) ;
#10879 = CARTESIAN_POINT ( 'NONE',  ( -9.987580305889029120, 184.1998911412988207, 323.1427045197882535 ) ) ;
#10880 = CARTESIAN_POINT ( 'NONE',  ( -91.18542874977060819, 79.95750479417183954, 31.50072335808886947 ) ) ;
#10881 = DIRECTION ( 'NONE',  ( -0.01292414190463832269, 0.000000000000000000, -0.9999164797902017066 ) ) ;
#10882 = ORIENTED_EDGE ( 'NONE', *, *, #3708, .T. ) ;
#10883 = CARTESIAN_POINT ( 'NONE',  ( 161.9999999999992610, 18.00000000000000355, 53.76161406891478123 ) ) ;
#10884 = ORIENTED_EDGE ( 'NONE', *, *, #7383, .F. ) ;
#10885 = DIRECTION ( 'NONE',  ( -0.1136178953597578312, 0.9935164314186356593, -0.004009283626633664867 ) ) ;
#10886 = CYLINDRICAL_SURFACE ( 'NONE', #12098, 6.499999999999985789 ) ;
#10887 = CARTESIAN_POINT ( 'NONE',  ( -14.85578608565897518, 180.2907807798002295, 316.9594776086723300 ) ) ;
#10888 = ORIENTED_EDGE ( 'NONE', *, *, #2365, .T. ) ;
#10889 = ORIENTED_EDGE ( 'NONE', *, *, #172, .T. ) ;
#10890 = DIRECTION ( 'NONE',  ( -0.9999164797902017066, 0.000000000000000000, 0.01292414190464117631 ) ) ;
#10891 = ADVANCED_FACE ( 'NONE', ( #17179 ), #11792, .F. ) ;
#10892 = ORIENTED_EDGE ( 'NONE', *, *, #12423, .T. ) ;
#10893 = CARTESIAN_POINT ( 'NONE',  ( 4.195452682864946325, 166.7895964344300808, 324.5942600080963985 ) ) ;
#10894 = EDGE_CURVE ( 'NONE', #4488, #4043, #12009, .T. ) ;
#10895 = CARTESIAN_POINT ( 'NONE',  ( -65.93268019054298179, 104.4142135623730923, -71.73965483371374319 ) ) ;
#10896 = FACE_OUTER_BOUND ( 'NONE', #18192, .T. ) ;
#10897 = DIRECTION ( 'NONE',  ( 0.9999164797902015955, 6.965998958219364448E-18, -0.01292414190464157182 ) ) ;
#10898 = EDGE_CURVE ( 'NONE', #16237, #12381, #11673, .T. ) ;
#10899 = VERTEX_POINT ( 'NONE', #8545 ) ;
#10900 = CARTESIAN_POINT ( 'NONE',  ( -55.33804461215960657, 114.2193244133317904, 167.6379947637574617 ) ) ;
#10901 = ORIENTED_EDGE ( 'NONE', *, *, #9991, .T. ) ;
#10902 = ADVANCED_FACE ( 'NONE', ( #18665 ), #20491, .F. ) ;
#10903 = CARTESIAN_POINT ( 'NONE',  ( 161.9999999999998579, 0.000000000000000000, -10.00000000000224176 ) ) ;
#10904 = VERTEX_POINT ( 'NONE', #17085 ) ;
#10905 = EDGE_LOOP ( 'NONE', ( #1943, #17430, #20509, #16984, #14329 ) ) ;
#10906 = CARTESIAN_POINT ( 'NONE',  ( 49.99582398951007889, 170.0000000000000284, -0.6462070952321007367 ) ) ;
#10907 =( NAMED_UNIT ( * ) SI_UNIT ( $, .STERADIAN. ) SOLID_ANGLE_UNIT ( ) );
#10908 = CARTESIAN_POINT ( 'NONE',  ( 45.19561618717597185, 127.3639955235004777, 246.9673780573190527 ) ) ;
#10909 = PLANE ( 'NONE',  #7635 ) ;
#10910 = CARTESIAN_POINT ( 'NONE',  ( 30.69487628741233465, 91.18588819953914992, 79.89877478592977411 ) ) ;
#10911 = EDGE_LOOP ( 'NONE', ( #10005, #10503, #9017, #13135 ) ) ;
#10912 = ORIENTED_EDGE ( 'NONE', *, *, #1346, .F. ) ;
#10913 = CARTESIAN_POINT ( 'NONE',  ( 20.28256946961299434, 148.9480170188545571, 278.4103539590889227 ) ) ;
#10914 = AXIS2_PLACEMENT_3D ( 'NONE', #10900, #17927, #7567 ) ;
#10915 = CARTESIAN_POINT ( 'NONE',  ( -8.517247419455044266, 185.4376447080673529, 305.5391571354516600 ) ) ;
#10916 = ADVANCED_FACE ( 'NONE', ( #2930 ), #18566, .T. ) ;
#10917 = VERTEX_POINT ( 'NONE', #10283 ) ;
#10918 = EDGE_CURVE ( 'NONE', #21383, #17288, #8227, .T. ) ;
#10919 = DIRECTION ( 'NONE',  ( 0.01292394549866738782, 0.005513023399720468239, 0.9999012842304692006 ) ) ;
#10920 = CARTESIAN_POINT ( 'NONE',  ( -89.94033328634043301, 88.81992964173861083, 52.36201159483771761 ) ) ;
#10921 = ADVANCED_FACE ( 'NONE', ( #8428 ), #15259, .T. ) ;
#10922 = SHAPE_REPRESENTATION ( 'Upper Movable Jaw Swivel Housing', ( #6292 ), #8126 ) ;
#10923 = DIRECTION ( 'NONE',  ( 0.9183650514339934956, 0.000000000000000000, -0.3957342950827467121 ) ) ;
#10924 = ORIENTED_EDGE ( 'NONE', *, *, #20023, .T. ) ;
#10925 = ORIENTED_EDGE ( 'NONE', *, *, #986, .T. ) ;
#10926 = CARTESIAN_POINT ( 'NONE',  ( 1.364373935098378649E-14, 105.0000000000000000, -9.836450281572198869E-15 ) ) ;
#10927 = CARTESIAN_POINT ( 'NONE',  ( 64.08803682720245831, 105.0000000000000000, -70.97692255680823337 ) ) ;
#10928 = CARTESIAN_POINT ( 'NONE',  ( -48.56673365018540522, 108.3817487785542824, -43.53692110109249569 ) ) ;
#10929 = CIRCLE ( 'NONE', #8337, 118.0000000000000000 ) ;
#10930 = CARTESIAN_POINT ( 'NONE',  ( 69.07678759757092735, 92.22190598759938496, -85.60612736256493349 ) ) ;
#10931 = VERTEX_POINT ( 'NONE', #16851 ) ;
#10932 = ADVANCED_FACE ( 'NONE', ( #8323 ), #6826, .F. ) ;
#10933 = CARTESIAN_POINT ( 'NONE',  ( 91.82493316891849133, 77.47293851758952599, 29.37406230631716397 ) ) ;
#10934 = VERTEX_POINT ( 'NONE', #20730 ) ;
#10935 = PLANE ( 'NONE',  #18761 ) ;
#10936 = CARTESIAN_POINT ( 'NONE',  ( -92.50752184771765485, 77.20349362929613335, -28.92971669647242905 ) ) ;
#10937 = FACE_OUTER_BOUND ( 'NONE', #1120, .T. ) ;
#10938 = CARTESIAN_POINT ( 'NONE',  ( -28.54471604494488446, 324.0454186304925202, 313.6477539799737428 ) ) ;
#10939 = PLANE ( 'NONE',  #3695 ) ;
#10940 = DIRECTION ( 'NONE',  ( 0.01292394549866739996, 0.005513023399721131770, 0.9999012842304692006 ) ) ;
#10941 = FACE_OUTER_BOUND ( 'NONE', #12522, .T. ) ;
#10942 = DIRECTION ( 'NONE',  ( 2.025474946048326158E-22, -1.000000000000000000, 1.876735158486679638E-22 ) ) ;
#10943 = CIRCLE ( 'NONE', #8713, 5.700000000000001954 ) ;
#10944 = ORIENTED_EDGE ( 'NONE', *, *, #7956, .T. ) ;
#10945 = ORIENTED_EDGE ( 'NONE', *, *, #18426, .F. ) ;
#10946 = CARTESIAN_POINT ( 'NONE',  ( -81.57403594986455175, 75.12325561942537888, 5.894141314586137881 ) ) ;
#10947 = AXIS2_PLACEMENT_3D ( 'NONE', #16438, #5680, #20965 ) ;
#10948 = CARTESIAN_POINT ( 'NONE',  ( 16.96733342230854902, 187.3721694870787076, 319.4512518112545649 ) ) ;
#10949 = EDGE_CURVE ( 'NONE', #20688, #564, #22104, .T. ) ;
#10950 = B_SPLINE_CURVE_WITH_KNOTS ( 'NONE', 3,
 ( #14571, #12958, #20041, #4194, #767, #9732, #11443, #7766, #16747, #14803 ),
 .UNSPECIFIED., .F., .F.,
 ( 4, 2, 2, 2, 4 ),
 ( 0.000000000000000000, 0.0004370559136044749457, 0.0008741118272089498913, 0.001311167740813424729, 0.001748223654417899783 ),
 .UNSPECIFIED. ) ;
#10951 = VERTEX_POINT ( 'NONE', #13630 ) ;
#10952 = CARTESIAN_POINT ( 'NONE',  ( -12.86548928906161571, 326.2291019854885121, 410.4442357137708086 ) ) ;
#10953 = CARTESIAN_POINT ( 'NONE',  ( -1.632550740186649252, 142.7036636415817838, 274.8672572718561469 ) ) ;
#10954 = CARTESIAN_POINT ( 'NONE',  ( -1.788039671088772931, 157.5463400564191545, 323.7224625657159436 ) ) ;
#10955 = FACE_OUTER_BOUND ( 'NONE', #22069, .T. ) ;
#10956 = ADVANCED_FACE ( 'NONE', ( #10168 ), #9284, .F. ) ;
#10957 = VECTOR ( 'NONE', #6464, 999.9999999999998863 ) ;
#10958 = EDGE_LOOP ( 'NONE', ( #11215, #15595, #5520, #4648 ) ) ;
#10959 = CARTESIAN_POINT ( 'NONE',  ( -10.01777582550143642, 187.9231991978160750, 308.1591746062594552 ) ) ;
#10960 = CARTESIAN_POINT ( 'NONE',  ( 18.16399122330053828, 185.9192657936563648, 277.9565842329805605 ) ) ;
#10961 = CARTESIAN_POINT ( 'NONE',  ( 14.48605119362585292, 189.3857847177796145, 308.1185926126519234 ) ) ;
#10962 = CARTESIAN_POINT ( 'NONE',  ( 91.41775219751511372, 77.84255103198131565, 29.95431514106030590 ) ) ;
#10963 = FACE_OUTER_BOUND ( 'NONE', #13066, .T. ) ;
#10964 = ORIENTED_EDGE ( 'NONE', *, *, #1017, .T. ) ;
#10965 =( LENGTH_UNIT ( ) NAMED_UNIT ( * ) SI_UNIT ( .MILLI., .METRE. ) );
#10966 = PLANE ( 'NONE',  #1512 ) ;
#10967 = DIRECTION ( 'NONE',  ( 0.01292394549866739996, 0.005513023399735009558, 0.9999012842304692006 ) ) ;
#10968 = ORIENTED_EDGE ( 'NONE', *, *, #17950, .F. ) ;
#10969 = CARTESIAN_POINT ( 'NONE',  ( -90.14522075562827297, 79.46791348803235167, -27.62924625256264122 ) ) ;
#10970 = AXIS2_PLACEMENT_3D ( 'NONE', #13437, #20519, #4779 ) ;
#10971 = ORIENTED_EDGE ( 'NONE', *, *, #18787, .T. ) ;
#10972 = EDGE_CURVE ( 'NONE', #530, #21215, #8556, .T. ) ;
#10973 = ADVANCED_FACE ( 'NONE', ( #5554 ), #14438, .F. ) ;
#10974 = AXIS2_PLACEMENT_3D ( 'NONE', #7690, #19970, #696 ) ;
#10975 = FACE_OUTER_BOUND ( 'NONE', #12318, .T. ) ;
#10976 = CARTESIAN_POINT ( 'NONE',  ( 45.73105848731719192, 168.8134312302534283, 56.26981079935081453 ) ) ;
#10977 = CARTESIAN_POINT ( 'NONE',  ( -92.40872671617950118, 72.00000000000000000, 33.19707612406966746 ) ) ;
#10978 = CARTESIAN_POINT ( 'NONE',  ( 79.25033911284278076, 75.20308137605636034, 5.185103052828717196 ) ) ;
#10979 = CARTESIAN_POINT ( 'NONE',  ( -55.72518630658383643, 88.80328459322107904, 164.8033799449534627 ) ) ;
#10980 = ORIENTED_EDGE ( 'NONE', *, *, #14843, .F. ) ;
#10981 = CARTESIAN_POINT ( 'NONE',  ( 12.16090316381096592, 187.7181452293938264, 322.9758963384301751 ) ) ;
#10982 = CARTESIAN_POINT ( 'NONE',  ( 118.1650300934700937, -0.6522510975647682896, -119.8463544630189404 ) ) ;
#10983 = LINE ( 'NONE', #7426, #19224 ) ;
#10984 = CIRCLE ( 'NONE', #1095, 9.000000000000003553 ) ;
#10985 = CARTESIAN_POINT ( 'NONE',  ( 71.43040806848138402, 92.41825753590681813, 83.65230687350620542 ) ) ;
#10986 = VECTOR ( 'NONE', #10208, 1000.000000000000114 ) ;
#10988 = DIRECTION ( 'NONE',  ( -0.01292394549866738608, -0.005513023399720699824, -0.9999012842304692006 ) ) ;
#10987 = CARTESIAN_POINT ( 'NONE',  ( -90.90077733783158465, 77.56213813822601821, 31.87679858714241021 ) ) ;
#10989 = PLANE ( 'NONE',  #18742 ) ;
#10990 = ORIENTED_EDGE ( 'NONE', *, *, #138, .F. ) ;
#10991 = CARTESIAN_POINT ( 'NONE',  ( -14.55445127856342680, 180.9963701914269336, 317.7651582568626054 ) ) ;
#10992 = DIRECTION ( 'NONE',  ( 0.000000000000000000, -0.005512562964840580192, -0.9999848057093461140 ) ) ;
#10993 = CARTESIAN_POINT ( 'NONE',  ( -15.09948650839594109, 178.4733586872830529, 317.9816280114638971 ) ) ;
#10994 = ORIENTED_EDGE ( 'NONE', *, *, #2126, .F. ) ;
#10995 = ORIENTED_EDGE ( 'NONE', *, *, #2688, .T. ) ;
#10996 = EDGE_CURVE ( 'NONE', #6260, #15641, #4526, .T. ) ;
#10997 = LINE ( 'NONE', #2046, #4022 ) ;
#10998 = ORIENTED_EDGE ( 'NONE', *, *, #19606, .T. ) ;
#10999 = AXIS2_PLACEMENT_3D ( 'NONE', #2745, #9755, #16769 ) ;
#11000 = VECTOR ( 'NONE', #1081, 1000.000000000000227 ) ;
#11001 = CARTESIAN_POINT ( 'NONE',  ( 12.36865781294890532, 189.2856407680814641, 307.5221633547453166 ) ) ;
#11002 = VECTOR ( 'NONE', #19605, 1000.000000000000114 ) ;
#11003 = ORIENTED_EDGE ( 'NONE', *, *, #12120, .F. ) ;
#11004 = DIRECTION ( 'NONE',  ( -0.7944560844389300103, 0.000000000000000000, -0.6073216033519338586 ) ) ;
#11005 = VECTOR ( 'NONE', #5123, 999.9999999999998863 ) ;
#11006 = CARTESIAN_POINT ( 'NONE',  ( 13.59252474903330210, 159.3044100855808836, 323.5139721269083566 ) ) ;
#11007 = ORIENTED_EDGE ( 'NONE', *, *, #15459, .F. ) ;
#11008 = ORIENTED_EDGE ( 'NONE', *, *, #9281, .T. ) ;
#11009 = CARTESIAN_POINT ( 'NONE',  ( -90.00000000000000000, 0.000000000000000000, 8.394090934816448357E-16 ) ) ;
#11010 = ADVANCED_FACE ( 'NONE', ( #15932 ), #19112, .F. ) ;
#11011 = VERTEX_POINT ( 'NONE', #16047 ) ;
#11012 = DIRECTION ( 'NONE',  ( 0.000000000000000000, -0.7071067811865465735, -0.7071067811865483499 ) ) ;
#11013 = VERTEX_POINT ( 'NONE', #10740 ) ;
#11014 = CARTESIAN_POINT ( 'NONE',  ( -12.58378492319879527, 109.7167104967248434, 130.3428598364639299 ) ) ;
#11015 = DIRECTION ( 'NONE',  ( 0.9999164797902015955, 6.965998958219364448E-18, -0.01292414190464157182 ) ) ;
#11016 = DIRECTION ( 'NONE',  ( -0.9999164797902015955, -2.219203356785934189E-15, 0.01292414190464157009 ) ) ;
#11017 = FACE_OUTER_BOUND ( 'NONE', #4904, .T. ) ;
#11018 = VECTOR ( 'NONE', #18433, 1000.000000000000000 ) ;
#11019 = VECTOR ( 'NONE', #2346, 1000.000000000000114 ) ;
#11020 = EDGE_LOOP ( 'NONE', ( #6745, #13208, #3463, #15541 ) ) ;
#11021 = LINE ( 'NONE', #19727, #6786 ) ;
#11022 = B_SPLINE_CURVE_WITH_KNOTS ( 'NONE', 3,
 ( #18857, #19196, #20568, #5170, #11866, #1415, #15436, #12210, #9908, #18961, #3006, #22390, #1195, #3220, #6469, #13480 ),
 .UNSPECIFIED., .F., .F.,
 ( 4, 2, 2, 2, 2, 2, 2, 4 ),
 ( 0.000000000000000000, 0.0004395957642550035564, 0.0008791915285100071129, 0.001758383057019986470, 0.002197978821274975281, 0.002637574585529963659, 0.003077170349784952470, 0.003516766114039940848 ),
 .UNSPECIFIED. ) ;
#11023 = ITEM_DEFINED_TRANSFORMATION ( 'NONE', 'NONE', #17651,  #6292 ) ;
#11024 = CYLINDRICAL_SURFACE ( 'NONE', #21962, 2.000000000000001332 ) ;
#11025 = VECTOR ( 'NONE', #1785, 1000.000000000000000 ) ;
#11026 = ORIENTED_EDGE ( 'NONE', *, *, #14305, .F. ) ;
#11027 = EDGE_CURVE ( 'NONE', #20773, #3794, #8202, .T. ) ;
#11028 = PLANE ( 'NONE',  #10610 ) ;
#11029 = DIRECTION ( 'NONE',  ( 0.000000000000000000, 0.000000000000000000, 1.000000000000000000 ) ) ;
#11030 = ADVANCED_FACE ( 'NONE', ( #12122 ), #5996, .T. ) ;
#11031 = DIRECTION ( 'NONE',  ( 0.000000000000000000, 0.000000000000000000, 1.000000000000000000 ) ) ;
#11032 = B_SPLINE_CURVE_WITH_KNOTS ( 'NONE', 3,
 ( #7259, #6605, #263, #5407, #5527, #3053, #12446, #12560, #17863, #9082, #8326, #15368, #20618, #11173, #608, #2441 ),
 .UNSPECIFIED., .F., .F.,
 ( 4, 2, 2, 2, 2, 2, 2, 4 ),
 ( -0.003151246785043320189, -0.002357650993505802130, -0.001960853097737045268, -0.001564055201968288624, -0.001167257306199531979, -0.0007704594104307751178, -0.0003736615146620182563, 2.313638110673860507E-05 ),
 .UNSPECIFIED. ) ;
#11033 = VECTOR ( 'NONE', #7493, 1000.000000000000000 ) ;
#11034 = ORIENTED_EDGE ( 'NONE', *, *, #632, .F. ) ;
#11035 = CIRCLE ( 'NONE', #1147, 26.23296215977917356 ) ;
#11036 = DIRECTION ( 'NONE',  ( 0.009760756503427994377, -0.9999378516499565217, 0.005387065077612505741 ) ) ;
#11037 = EDGE_LOOP ( 'NONE', ( #5804, #11246, #905, #5386, #5973, #4287 ) ) ;
#11038 = DIRECTION ( 'NONE',  ( 0.000000000000000000, -1.000000000000000000, 0.000000000000000000 ) ) ;
#11039 = CIRCLE ( 'NONE', #5884, 9.000000000000001776 ) ;
#11040 = DIRECTION ( 'NONE',  ( 0.01292394549866738261, 0.005513023399722618428, 0.9999012842304692006 ) ) ;
#11041 = EDGE_CURVE ( 'NONE', #9056, #10110, #17476, .T. ) ;
#11042 = CARTESIAN_POINT ( 'NONE',  ( -105.9308899693960484, 70.24357031783570449, -29.64301131075929518 ) ) ;
#11043 = CARTESIAN_POINT ( 'NONE',  ( -45.96244189366829858, 171.4878726268958360, -74.17150848012535391 ) ) ;
#11044 = EDGE_CURVE ( 'NONE', #1720, #20978, #10514, .T. ) ;
#11045 = EDGE_LOOP ( 'NONE', ( #14579, #11189, #11231, #21664 ) ) ;
#11046 = CYLINDRICAL_SURFACE ( 'NONE', #11728, 11.00000000000000178 ) ;
#11047 = AXIS2_PLACEMENT_3D ( 'NONE', #551, #12392, #14232 ) ;
#11048 = EDGE_LOOP ( 'NONE', ( #10823, #10656, #6506, #3693, #14728, #635 ) ) ;
#11049 = DIRECTION ( 'NONE',  ( -0.000000000000000000, -1.000000000000000000, -0.000000000000000000 ) ) ;
#11050 = EDGE_CURVE ( 'NONE', #8794, #13983, #5438, .T. ) ;
#11051 = CARTESIAN_POINT ( 'NONE',  ( 50.40347573247742474, 189.6005870223182228, -73.16055181083503101 ) ) ;
#11052 = CARTESIAN_POINT ( 'NONE',  ( -17.63692254078916832, 314.5473693806632127, 324.2384804942064989 ) ) ;
#11053 = FACE_BOUND ( 'NONE', #6847, .T. ) ;
#11054 = DIRECTION ( 'NONE',  ( -0.01292394549866741384, -0.005513023399721131770, -0.9999012842304692006 ) ) ;
#11055 = EDGE_CURVE ( 'NONE', #8554, #14680, #6017, .T. ) ;
#11056 = ORIENTED_EDGE ( 'NONE', *, *, #6468, .T. ) ;
#11057 = CYLINDRICAL_SURFACE ( 'NONE', #10011, 2.009999999999995346 ) ;
#11058 = PLANE ( 'NONE',  #13414 ) ;
#11059 = CARTESIAN_POINT ( 'NONE',  ( 40.48953805856821475, 105.9808811061030553, 91.99283320860411095 ) ) ;
#11060 = ORIENTED_EDGE ( 'NONE', *, *, #5387, .T. ) ;
#11061 = AXIS2_PLACEMENT_3D ( 'NONE', #2359, #13063, #21618 ) ;
#11062 = DIRECTION ( 'NONE',  ( 5.440186201345785633E-18, 1.000000000000000000, 1.334940939666367878E-17 ) ) ;
#11063 = VECTOR ( 'NONE', #9550, 1000.000000000000000 ) ;
#11064 = VERTEX_POINT ( 'NONE', #14660 ) ;
#11065 = AXIS2_PLACEMENT_3D ( 'NONE', #12807, #19780, #8076 ) ;
#11066 = CARTESIAN_POINT ( 'NONE',  ( -84.84767091729572996, 75.01394013563931651, -0.5387156272771348453 ) ) ;
#11067 = CARTESIAN_POINT ( 'NONE',  ( -88.16184267143731290, 88.07739181906583781, 53.04568397887596376 ) ) ;
#11068 = ADVANCED_FACE ( 'NONE', ( #13054 ), #17018, .T. ) ;
#11069 = CIRCLE ( 'NONE', #14766, 3.399999999999985700 ) ;
#11071 = EDGE_LOOP ( 'NONE', ( #7012, #3887, #14716, #14163 ) ) ;
#11070 = EDGE_LOOP ( 'NONE', ( #18583, #6459, #18896, #18677 ) ) ;
#11072 = CARTESIAN_POINT ( 'NONE',  ( 40.14615270801867553, 95.25460127842278268, -44.16447546512498690 ) ) ;
#11073 = CARTESIAN_POINT ( 'NONE',  ( -2.931228531347772392, 143.0481234405170028, 275.4479384761518190 ) ) ;
#11074 = VECTOR ( 'NONE', #17589, 999.9999999999998863 ) ;
#11075 = CARTESIAN_POINT ( 'NONE',  ( -39.45590449607104944, 92.86731729158431392, -83.62973377257371510 ) ) ;
#11076 = CONICAL_SURFACE ( 'NONE', #22406, 5.010000000000001563, 0.9599310885968744822 ) ;
#11077 = LINE ( 'NONE', #9346, #13725 ) ;
#11078 = DIRECTION ( 'NONE',  ( -0.01292394549866740863, -0.005513023399721176006, -0.9999012842304692006 ) ) ;
#11079 = LINE ( 'NONE', #12702, #1249 ) ;
#11080 = CIRCLE ( 'NONE', #17311, 2.000000000000001332 ) ;
#11081 = CARTESIAN_POINT ( 'NONE',  ( 19.82458506650596419, 183.6531909117268526, 313.2672148072155096 ) ) ;
#11082 = FACE_OUTER_BOUND ( 'NONE', #19677, .T. ) ;
#11083 = CARTESIAN_POINT ( 'NONE',  ( 1.364374644014609697E-14, 69.99999999999998579, -9.836443712999143722E-15 ) ) ;
#11084 = EDGE_CURVE ( 'NONE', #198, #13705, #627, .T. ) ;
#11085 = ORIENTED_EDGE ( 'NONE', *, *, #21292, .F. ) ;
#11086 = AXIS2_PLACEMENT_3D ( 'NONE', #4946, #15551, #14049 ) ;
#11087 = DIRECTION ( 'NONE',  ( -7.125109674381880655E-05, 0.9999848031710252272, -0.005512562950849702291 ) ) ;
#11088 = FACE_OUTER_BOUND ( 'NONE', #11272, .T. ) ;
#11089 = VERTEX_POINT ( 'NONE', #9348 ) ;
#11091 = LINE ( 'NONE', #9464, #9102 ) ;
#11090 = CIRCLE ( 'NONE', #15160, 6.499999999999985789 ) ;
#11092 = ORIENTED_EDGE ( 'NONE', *, *, #19061, .T. ) ;
#11093 = ORIENTED_EDGE ( 'NONE', *, *, #1948, .T. ) ;
#11094 = VECTOR ( 'NONE', #2502, 999.9999999999998863 ) ;
#11095 = AXIS2_PLACEMENT_3D ( 'NONE', #16074, #12389, #14346 ) ;
#11096 = CARTESIAN_POINT ( 'NONE',  ( 2.809107650776963450, 87.00000000000001421, -86.95587516435855946 ) ) ;
#11097 = ADVANCED_FACE ( 'NONE', ( #19669 ), #12805, .T. ) ;
#11098 = CARTESIAN_POINT ( 'NONE',  ( 41.22233984835247611, 119.7725967263615985, 249.0607866758211344 ) ) ;
#11099 = AXIS2_PLACEMENT_3D ( 'NONE', #16694, #6203, #9878 ) ;
#11100 = DIRECTION ( 'NONE',  ( 0.4397038457472424167, 0.000000000000000000, -0.8981428216242032248 ) ) ;
#11101 = CARTESIAN_POINT ( 'NONE',  ( 70.91392079944854743, 91.17157287525388654, 84.09052168258639881 ) ) ;
#11102 = CARTESIAN_POINT ( 'NONE',  ( -55.40268456415261511, 20.00000000000000000, 113.1659955246496025 ) ) ;
#11103 = CARTESIAN_POINT ( 'NONE',  ( -22.49358496127894824, 324.7653478115763050, 320.5678661935266973 ) ) ;
#11104 = DIRECTION ( 'NONE',  ( 7.125109674159588039E-05, -0.9999848031710253382, 0.005512562950848870491 ) ) ;
#11105 = ORIENTED_EDGE ( 'NONE', *, *, #19314, .F. ) ;
#11106 = DIRECTION ( 'NONE',  ( 0.01292394549866771568, 0.005513023399718815047, 0.9999012842304693116 ) ) ;
#11107 = ORIENTED_EDGE ( 'NONE', *, *, #17945, .F. ) ;
#11108 = CARTESIAN_POINT ( 'NONE',  ( 0.000000000000000000, 0.000000000000000000, 0.000000000000000000 ) ) ;
#11109 = AXIS2_PLACEMENT_3D ( 'NONE', #8566, #8447, #15497 ) ;
#11110 = DIRECTION ( 'NONE',  ( 0.9999164797902017066, 6.965998958219365988E-18, -0.01292414190464157356 ) ) ;
#11111 = AXIS2_PLACEMENT_3D ( 'NONE', #21981, #8231, #6282 ) ;
#11112 = CARTESIAN_POINT ( 'NONE',  ( 92.16545979397402277, 77.13735158510392864, -31.20743466190268833 ) ) ;
#11113 = EDGE_CURVE ( 'NONE', #20395, #3828, #20296, .T. ) ;
#11114 = FACE_BOUND ( 'NONE', #7693, .T. ) ;
#11115 = ADVANCED_FACE ( 'NONE', ( #2696 ), #2224, .T. ) ;
#11116 = CARTESIAN_POINT ( 'NONE',  ( -92.19651396575542890, 79.04398536194661062, 28.61663131200403498 ) ) ;
#11117 = DIRECTION ( 'NONE',  ( -0.01292394549866750231, -0.005513023399722823126, -0.9999012842304692006 ) ) ;
#11118 = ORIENTED_EDGE ( 'NONE', *, *, #18556, .T. ) ;
#11119 = CARTESIAN_POINT ( 'NONE',  ( -44.75523122589896019, 161.1026720614313774, 19.22810367108447238 ) ) ;
#11120 = ORIENTED_EDGE ( 'NONE', *, *, #20722, .F. ) ;
#11121 = DIRECTION ( 'NONE',  ( -0.009188991635466050092, 0.7031977391749439921, -0.7109349492407662785 ) ) ;
#11122 = AXIS2_PLACEMENT_3D ( 'NONE', #16766, #14824, #4323 ) ;
#11123 = CARTESIAN_POINT ( 'NONE',  ( -10.01711797457082831, 184.3274371752771685, 305.4743107222549270 ) ) ;
#11124 = VERTEX_POINT ( 'NONE', #2574 ) ;
#11125 = ORIENTED_EDGE ( 'NONE', *, *, #4242, .F. ) ;
#11126 = DIRECTION ( 'NONE',  ( -0.01292394549866632963, -0.005513023399716958026, -0.9999012842304692006 ) ) ;
#11127 = AXIS2_PLACEMENT_3D ( 'NONE', #6498, #12005, #9941 ) ;
#11128 = DIRECTION ( 'NONE',  ( 0.01292414190464131335, 1.902755938799530239E-22, 0.9999164797902015955 ) ) ;
#11129 = ORIENTED_EDGE ( 'NONE', *, *, #9063, .F. ) ;
#11130 = FACE_OUTER_BOUND ( 'NONE', #6739, .T. ) ;
#11131 = LINE ( 'NONE', #13096, #18703 ) ;
#11132 = VERTEX_POINT ( 'NONE', #973 ) ;
#11133 = AXIS2_PLACEMENT_3D ( 'NONE', #16158, #21399, #12466 ) ;
#11134 = EDGE_LOOP ( 'NONE', ( #16838, #16505, #8972, #21453 ) ) ;
#11135 = FACE_OUTER_BOUND ( 'NONE', #3124, .T. ) ;
#11136 = DIRECTION ( 'NONE',  ( -0.9999164797902015955, 0.000000000000000000, 0.01292414190464162733 ) ) ;
#11137 = CARTESIAN_POINT ( 'NONE',  ( -50.34903424743296796, 95.63295186387540525, -44.50339194506212692 ) ) ;
#11138 = ORIENTED_EDGE ( 'NONE', *, *, #4440, .F. ) ;
#11139 = LINE ( 'NONE', #2847, #11820 ) ;
#11140 = ORIENTED_EDGE ( 'NONE', *, *, #8863, .F. ) ;
#11141 = DIRECTION ( 'NONE',  ( -1.000000000000000000, 0.000000000000000000, 0.000000000000000000 ) ) ;
#11142 = FACE_OUTER_BOUND ( 'NONE', #2416, .T. ) ;
#11143 = LINE ( 'NONE', #19962, #5931 ) ;
#11144 = CIRCLE ( 'NONE', #8207, 21.67179167071592261 ) ;
#11145 = ORIENTED_EDGE ( 'NONE', *, *, #18345, .T. ) ;
#11146 = AXIS2_PLACEMENT_3D ( 'NONE', #19450, #13951, #15689 ) ;
#11147 = DIRECTION ( 'NONE',  ( 0.01292394549866739996, 0.005513023399721131770, 0.9999012842304692006 ) ) ;
#11148 = DIRECTION ( 'NONE',  ( -0.01292394549866632963, -0.005513023399716958026, -0.9999012842304692006 ) ) ;
#11149 = EDGE_LOOP ( 'NONE', ( #6024, #4378, #10812, #2711 ) ) ;
#11150 = CIRCLE ( 'NONE', #5643, 10.00000000000001421 ) ;
#11151 = CARTESIAN_POINT ( 'NONE',  ( 11.85964614693714836, 187.7423844643599296, 304.8777488482054423 ) ) ;
#11152 = CARTESIAN_POINT ( 'NONE',  ( -89.85439142418879044, 87.94879146495189559, 50.81774004189161076 ) ) ;
#11153 = APPLICATION_PROTOCOL_DEFINITION ( 'draft international standard', 'automotive_design', 1998, #2212 ) ;
#11154 = ORIENTED_EDGE ( 'NONE', *, *, #17341, .F. ) ;
#11155 = AXIS2_PLACEMENT_3D ( 'NONE', #15398, #9986, #7915 ) ;
#11156 = DIRECTION ( 'NONE',  ( -0.01292394549866737220, -0.005513023399721000799, -0.9999012842304692006 ) ) ;
#11157 = ORIENTED_EDGE ( 'NONE', *, *, #170, .T. ) ;
#11158 = DIRECTION ( 'NONE',  ( -0.9999164797902015955, -2.001050586450178695E-22, 0.01292414190464131335 ) ) ;
#11159 = DIRECTION ( 'NONE',  ( -1.000000000000000000, 0.000000000000000000, 0.000000000000000000 ) ) ;
#11160 = DIRECTION ( 'NONE',  ( -0.01292394549866738782, -0.005513023399720468239, -0.9999012842304692006 ) ) ;
#11161 = CARTESIAN_POINT ( 'NONE',  ( -35.39322062607227792, 92.77591188308414871, 83.66707218845635907 ) ) ;
#11162 = ORIENTED_EDGE ( 'NONE', *, *, #18266, .T. ) ;
#11163 = DIRECTION ( 'NONE',  ( -0.01292394549866739996, -0.005513023399721131770, -0.9999012842304692006 ) ) ;
#11164 = ORIENTED_EDGE ( 'NONE', *, *, #11817, .F. ) ;
#11165 = DIRECTION ( 'NONE',  ( 0.01292394549866728373, 0.005513023399720296501, 0.9999012842304693116 ) ) ;
#11166 = CARTESIAN_POINT ( 'NONE',  ( 50.53293774634011726, 189.6008146261148113, -73.12093756438817138 ) ) ;
#11167 = AXIS2_PLACEMENT_3D ( 'NONE', #13989, #1586, #5350 ) ;
#11168 = DIRECTION ( 'NONE',  ( 5.440186201345738641E-18, 1.000000000000000000, 1.334940939666364181E-17 ) ) ;
#11169 = DIRECTION ( 'NONE',  ( 0.000000000000000000, 0.000000000000000000, 1.000000000000000000 ) ) ;
#11170 = EDGE_CURVE ( 'NONE', #7316, #9279, #5626, .T. ) ;
#11171 = SPHERICAL_SURFACE ( 'NONE', #13253, 2.000000000000000000 ) ;
#11172 = VERTEX_POINT ( 'NONE', #4052 ) ;
#11173 = CARTESIAN_POINT ( 'NONE',  ( -40.81696164862506038, 106.8158423209496135, 71.47546216999431579 ) ) ;
#11174 = EDGE_CURVE ( 'NONE', #3247, #1930, #11079, .T. ) ;
#11175 = DIRECTION ( 'NONE',  ( 0.9999164797902015955, 6.965998958219364448E-18, -0.01292414190464157182 ) ) ;
#11176 = EDGE_LOOP ( 'NONE', ( #1513, #38, #14935, #3776 ) ) ;
#11177 = AXIS2_PLACEMENT_3D ( 'NONE', #19149, #14004, #8684 ) ;
#11178 = DIRECTION ( 'NONE',  ( -0.7944560844389304544, 0.000000000000000000, -0.6073216033519334145 ) ) ;
#11179 = CARTESIAN_POINT ( 'NONE',  ( -1.163172771417702478, 87.00000000000001421, -89.99248318111824574 ) ) ;
#11180 = EDGE_LOOP ( 'NONE', ( #4944, #12558, #4991, #15124 ) ) ;
#11181 = VERTEX_POINT ( 'NONE', #7618 ) ;
#11182 =( REPRESENTATION_RELATIONSHIP ('NONE','NONE', #11808, #5468 ) REPRESENTATION_RELATIONSHIP_WITH_TRANSFORMATION ( #3188 )SHAPE_REPRESENTATION_RELATIONSHIP( ) );
#11183 = ADVANCED_FACE ( 'NONE', ( #2457 ), #18307, .T. ) ;
#11184 = CARTESIAN_POINT ( 'NONE',  ( -90.16570127241018895, 87.17484075746328642, 51.29199764768473813 ) ) ;
#11185 = EDGE_CURVE ( 'NONE', #17187, #14649, #13365, .T. ) ;
#11186 = CIRCLE ( 'NONE', #17068, 2.999999999999999556 ) ;
#11188 = ORIENTED_EDGE ( 'NONE', *, *, #18607, .T. ) ;
#11187 = EDGE_LOOP ( 'NONE', ( #10252, #4954, #4839, #17601, #16613, #11912 ) ) ;
#11189 = ORIENTED_EDGE ( 'NONE', *, *, #7145, .F. ) ;
#11190 = EDGE_CURVE ( 'NONE', #13521, #12879, #13692, .T. ) ;
#11191 = FACE_OUTER_BOUND ( 'NONE', #20256, .T. ) ;
#11192 = FACE_OUTER_BOUND ( 'NONE', #4709, .T. ) ;
#11193 = AXIS2_PLACEMENT_3D ( 'NONE', #6533, #20763, #3187 ) ;
#11194 = CARTESIAN_POINT ( 'NONE',  ( -89.40819020483021973, 79.89452498912720557, -28.94780723987650362 ) ) ;
#11195 = CARTESIAN_POINT ( 'NONE',  ( -64.64767546932813502, 126.1473081376430798, 27.67873648630093797 ) ) ;
#11196 = VERTEX_POINT ( 'NONE', #6695 ) ;
#11197 = LINE ( 'NONE', #397, #19073 ) ;
#11198 = DIRECTION ( 'NONE',  ( 0.01292414190465215537, 0.000000000000000000, 0.9999164797902015955 ) ) ;
#11199 = CARTESIAN_POINT ( 'NONE',  ( 20.63696371470829760, 181.9335396870980048, 313.3533115342202677 ) ) ;
#11200 = CARTESIAN_POINT ( 'NONE',  ( 5.208897394599592445, 86.29861661753390933, -75.24359988578153491 ) ) ;
#11201 = EDGE_CURVE ( 'NONE', #16990, #13823, #6579, .T. ) ;
#11202 = ADVANCED_FACE ( 'NONE', ( #15109 ), #18641, .T. ) ;
#11203 = CARTESIAN_POINT ( 'NONE',  ( -54.52327687265816536, 2.000000000000000000, -111.3697098814011923 ) ) ;
#11204 =( BOUNDED_CURVE ( )  B_SPLINE_CURVE ( 3, ( #11913, #21377, #13636, #3821 ),
 .UNSPECIFIED., .F., .T. ) 
 B_SPLINE_CURVE_WITH_KNOTS ( ( 4, 4 ),
 ( 0.6960171423055208084, 0.7385976378458812830 ),
 .UNSPECIFIED. ) 
 CURVE ( )  GEOMETRIC_REPRESENTATION_ITEM ( )  RATIONAL_B_SPLINE_CURVE ( ( 1.000000000000000000, 0.9998489141570392480, 0.9998489141570392480, 1.000000000000000000 ) ) 
 REPRESENTATION_ITEM ( '' )  );
#11205 = EDGE_CURVE ( 'NONE', #17825, #7434, #19917, .T. ) ;
#11206 = PRODUCT_DEFINITION_SHAPE ( 'NONE', 'NONE',  #2137 ) ;
#11207 = CARTESIAN_POINT ( 'NONE',  ( -90.82246629754759226, 169.9999999999999716, 1.173900486973951773 ) ) ;
#11208 = CARTESIAN_POINT ( 'NONE',  ( -50.56880203129856000, 139.7551263635817236, -43.68402316449832057 ) ) ;
#11209 = ORIENTED_EDGE ( 'NONE', *, *, #2179, .F. ) ;
#11210 = CARTESIAN_POINT ( 'NONE',  ( 0.000000000000000000, 1.999999999999998224, 0.000000000000000000 ) ) ;
#11211 = ORIENTED_EDGE ( 'NONE', *, *, #21203, .F. ) ;
#11212 = EDGE_CURVE ( 'NONE', #8826, #12249, #3452, .T. ) ;
#11213 = CARTESIAN_POINT ( 'NONE',  ( -9.826031587490524188, 187.7354486172501709, 321.1602828553623681 ) ) ;
#11214 = EDGE_CURVE ( 'NONE', #16088, #2091, #16825, .T. ) ;
#11215 = ORIENTED_EDGE ( 'NONE', *, *, #14926, .F. ) ;
#11216 = EDGE_CURVE ( 'NONE', #9339, #16395, #8201, .T. ) ;
#11217 = CARTESIAN_POINT ( 'NONE',  ( 76.67480597215256921, 75.07749829403637420, 2.852969916228293101 ) ) ;
#11218 = CARTESIAN_POINT ( 'NONE',  ( -89.89473308095314508, 71.83810385978752322, 62.23413549537023215 ) ) ;
#11219 = CONICAL_SURFACE ( 'NONE', #2425, 9.000000000000001776, 1.047197551196594301 ) ;
#11220 = CARTESIAN_POINT ( 'NONE',  ( 77.29073663370949987, 75.16594760505751083, 4.616381533551536798 ) ) ;
#11221 = CARTESIAN_POINT ( 'NONE',  ( -7.337194850064199692, 109.6999844229167564, 127.2409188565385421 ) ) ;
#11222 = ORIENTED_EDGE ( 'NONE', *, *, #4772, .T. ) ;
#11223 = DIRECTION ( 'NONE',  ( 0.000000000000000000, 0.000000000000000000, 1.000000000000000000 ) ) ;
#11224 = CARTESIAN_POINT ( 'NONE',  ( 90.02055463237802257, 95.71211110526448351, -63.21629334023823077 ) ) ;
#11225 = CYLINDRICAL_SURFACE ( 'NONE', #7132, 6.500000000000000000 ) ;
#11226 = EDGE_CURVE ( 'NONE', #19373, #11778, #6831, .T. ) ;
#11227 = FACE_OUTER_BOUND ( 'NONE', #16117, .T. ) ;
#11228 = CARTESIAN_POINT ( 'NONE',  ( -8.630726460828782365, 185.9406206071954841, 321.2368171913553283 ) ) ;
#11229 = CARTESIAN_POINT ( 'NONE',  ( -90.81765045018502747, 77.62753381201262926, 31.97827203367538473 ) ) ;
#11230 = PRESENTATION_STYLE_ASSIGNMENT (( #18760 ) ) ;
#11231 = ORIENTED_EDGE ( 'NONE', *, *, #2473, .T. ) ;
#11232 = CARTESIAN_POINT ( 'NONE',  ( -54.52327687265816536, 0.000000000000000000, -111.3697098814011923 ) ) ;
#11233 = VERTEX_POINT ( 'NONE', #13493 ) ;
#11234 = ORIENTED_EDGE ( 'NONE', *, *, #14367, .T. ) ;
#11235 = CARTESIAN_POINT ( 'NONE',  ( -34.79726985247908999, 121.2962013336460814, 248.0347590154626971 ) ) ;
#11236 = CARTESIAN_POINT ( 'NONE',  ( -14.82189735930671759, 179.0281877771801931, 312.6327372929670219 ) ) ;
#11237 = ORIENTED_EDGE ( 'NONE', *, *, #11214, .T. ) ;
#11238 = VECTOR ( 'NONE', #7825, 1000.000000000000114 ) ;
#11239 = CARTESIAN_POINT ( 'NONE',  ( -14.19665567542432072, 325.6612605753163621, 307.4544034380322728 ) ) ;
#11240 = ORIENTED_EDGE ( 'NONE', *, *, #13853, .F. ) ;
#11241 = CARTESIAN_POINT ( 'NONE',  ( 12.31224524591022274, 189.1288638982456973, 307.4294852416394974 ) ) ;
#11242 = EDGE_CURVE ( 'NONE', #309, #17948, #10150, .T. ) ;
#11243 = CARTESIAN_POINT ( 'NONE',  ( 38.89810712971356566, 72.00000000000000000, -85.50986645835283184 ) ) ;
#11244 = CARTESIAN_POINT ( 'NONE',  ( 9.142505149400571796, 70.80384757729338219, -88.65345271381767134 ) ) ;
#11245 = VERTEX_POINT ( 'NONE', #15449 ) ;
#11246 = ORIENTED_EDGE ( 'NONE', *, *, #6536, .T. ) ;
#11247 = CARTESIAN_POINT ( 'NONE',  ( -92.40872671617950118, 34.61572286322119396, 33.19707612406966746 ) ) ;
#11248 = DIRECTION ( 'NONE',  ( -0.01292394549866704608, -0.005513023399720698957, -0.9999012842304692006 ) ) ;
#11249 = CARTESIAN_POINT ( 'NONE',  ( -15.48725902187971215, 177.8900859623065571, 313.3020055068878946 ) ) ;
#11250 = ORIENTED_EDGE ( 'NONE', *, *, #5603, .T. ) ;
#11251 = CARTESIAN_POINT ( 'NONE',  ( -106.7989984338461937, 79.11557862755601889, -26.34385626240375444 ) ) ;
#11252 =( NAMED_UNIT ( * ) SI_UNIT ( $, .STERADIAN. ) SOLID_ANGLE_UNIT ( ) );
#11253 = CARTESIAN_POINT ( 'NONE',  ( 12.66771380998468821, 189.3290151587127355, 321.0882186569899659 ) ) ;
#11254 = CARTESIAN_POINT ( 'NONE',  ( -40.63773027173701280, 95.80343475218985816, -42.17386218167892764 ) ) ;
#11255 = CARTESIAN_POINT ( 'NONE',  ( -33.82085273160089400, 93.50464841319747222, 82.93470554904384073 ) ) ;
#11256 = ORIENTED_EDGE ( 'NONE', *, *, #6195, .T. ) ;
#11257 = CARTESIAN_POINT ( 'NONE',  ( 51.99565694909076541, 169.9999999999999716, -0.6720553790413538175 ) ) ;
#11258 = CARTESIAN_POINT ( 'NONE',  ( 1.989200010245318451, 81.44091995301859299, -80.50723945831674655 ) ) ;
#11259 = ORIENTED_EDGE ( 'NONE', *, *, #2400, .F. ) ;
#11260 = DIRECTION ( 'NONE',  ( 0.8981428216242028917, -0.000000000000000000, -0.4397038457472432493 ) ) ;
#11261 = CARTESIAN_POINT ( 'NONE',  ( -88.17496191764027458, 88.96312264442134676, 51.79368639984505762 ) ) ;
#11262 = EDGE_CURVE ( 'NONE', #4456, #10097, #11326, .T. ) ;
#11263 = EDGE_CURVE ( 'NONE', #22552, #18970, #20246, .T. ) ;
#11264 = ORIENTED_EDGE ( 'NONE', *, *, #6679, .T. ) ;
#11265 = CARTESIAN_POINT ( 'NONE',  ( -52.56676294784124792, 113.4816418249608034, -43.51333844217711544 ) ) ;
#11266 = VERTEX_POINT ( 'NONE', #4624 ) ;
#11267 = CYLINDRICAL_SURFACE ( 'NONE', #21327, 2.000000000000000000 ) ;
#11268 = DIRECTION ( 'NONE',  ( 7.125109674161246868E-05, -0.9999848031710252272, 0.005512562950850154186 ) ) ;
#11269 = CARTESIAN_POINT ( 'NONE',  ( -106.0939156777172769, 70.76422767839098071, -29.05317630099631288 ) ) ;
#11270 = DIRECTION ( 'NONE',  ( 0.4768814951561130555, 0.000000000000000000, 0.8789675987075236119 ) ) ;
#11271 = DIRECTION ( 'NONE',  ( 0.000000000000000000, 0.000000000000000000, 1.000000000000000000 ) ) ;
#11272 = EDGE_LOOP ( 'NONE', ( #5638, #5119, #14342, #2392 ) ) ;
#11273 = CARTESIAN_POINT ( 'NONE',  ( 38.82295403925315469, 92.04141378167194887, -85.46747784716957597 ) ) ;
#11274 = CYLINDRICAL_SURFACE ( 'NONE', #8007, 96.00000000000000000 ) ;
#11275 = VERTEX_POINT ( 'NONE', #18752 ) ;
#11276 = DIRECTION ( 'NONE',  ( 0.9235411807339423129, 0.002179866145371284376, 0.3834930712179087098 ) ) ;
#11277 = CARTESIAN_POINT ( 'NONE',  ( -91.82493316891843449, 77.47293851758952599, -29.37406230631722082 ) ) ;
#11278 = LINE ( 'NONE', #5868, #2841 ) ;
#11279 = CARTESIAN_POINT ( 'NONE',  ( -7.853344289118919797, 165.3457450004224540, 308.2494022372945324 ) ) ;
#11280 = AXIS2_PLACEMENT_3D ( 'NONE', #7253, #9427, #605 ) ;
#11281 = DIRECTION ( 'NONE',  ( 0.8789675987075231678, 8.853465811791729457E-23, -0.4768814951561137772 ) ) ;
#11282 = CARTESIAN_POINT ( 'NONE',  ( 3.072605476372664679, 191.4131571344979932, 256.4662960534838589 ) ) ;
#11283 = CARTESIAN_POINT ( 'NONE',  ( -50.59241450076314806, 108.3707227317548529, -45.51087538574414992 ) ) ;
#11284 = VERTEX_POINT ( 'NONE', #3019 ) ;
#11285 = LINE ( 'NONE', #5875, #297 ) ;
#11286 = ORIENTED_EDGE ( 'NONE', *, *, #91, .F. ) ;
#11287 = VERTEX_POINT ( 'NONE', #18544 ) ;
#11288 = CARTESIAN_POINT ( 'NONE',  ( -82.74895026642346352, 75.09868225356439098, -3.260777892351517160 ) ) ;
#11289 = EDGE_CURVE ( 'NONE', #9564, #9131, #1986, .T. ) ;
#11290 = CARTESIAN_POINT ( 'NONE',  ( -90.15234812386498220, 88.12764344393974625, 53.04178249888710184 ) ) ;
#11291 = EDGE_CURVE ( 'NONE', #7202, #18705, #8303, .T. ) ;
#11292 = ORIENTED_EDGE ( 'NONE', *, *, #2056, .T. ) ;
#11293 = AXIS2_PLACEMENT_3D ( 'NONE', #1051, #22038, #6341 ) ;
#11294 = AXIS2_PLACEMENT_3D ( 'NONE', #3469, #12430, #10483 ) ;
#11295 = PLANE ( 'NONE',  #15874 ) ;
#11296 = FACE_OUTER_BOUND ( 'NONE', #9164, .T. ) ;
#11297 = CARTESIAN_POINT ( 'NONE',  ( -40.65822637310712651, 91.17157287525390075, -84.25167897319538213 ) ) ;
#11298 = B_SPLINE_CURVE_WITH_KNOTS ( 'NONE', 3,
 ( #4480, #4595, #9785, #9887, #20672, #16910, #16702, #1177 ),
 .UNSPECIFIED., .F., .F.,
 ( 4, 2, 2, 4 ),
 ( 0.002383014531731640628, 0.01915976248411578250, 0.02754813646030784824, 0.03593651043649991050 ),
 .UNSPECIFIED. ) ;
#11299 = CARTESIAN_POINT ( 'NONE',  ( 69.49687660543776246, 70.17287388826144934, 85.26604680535983505 ) ) ;
#11300 = VERTEX_POINT ( 'NONE', #20583 ) ;
#11301 = ORIENTED_EDGE ( 'NONE', *, *, #11514, .T. ) ;
#11302 = DIRECTION ( 'NONE',  ( -2.025474946048326158E-22, 1.000000000000000000, -1.876735158486679638E-22 ) ) ;
#11303 = CARTESIAN_POINT ( 'NONE',  ( 41.12105953731187924, 69.99999999999998579, 86.47576806556189410 ) ) ;
#11304 = CARTESIAN_POINT ( 'NONE',  ( 19.47897356911659728, 183.1989695422251145, 316.9366591568934837 ) ) ;
#11305 = FACE_OUTER_BOUND ( 'NONE', #3854, .T. ) ;
#11306 = AXIS2_PLACEMENT_3D ( 'NONE', #20346, #13367, #8384 ) ;
#11307 = ADVANCED_FACE ( 'NONE', ( #4841 ), #17035, .T. ) ;
#11308 = DIRECTION ( 'NONE',  ( -0.9999164797902015955, -2.457859219970326020E-15, 0.01292414190464043211 ) ) ;
#11309 = ORIENTED_EDGE ( 'NONE', *, *, #21123, .F. ) ;
#11310 =( NAMED_UNIT ( * ) PLANE_ANGLE_UNIT ( ) SI_UNIT ( $, .RADIAN. ) );
#11311 = APPLICATION_CONTEXT ( 'automotive_design' ) ;
#11312 = CARTESIAN_POINT ( 'NONE',  ( -36.80549447617401881, 105.5072037373731888, 92.66220808178287882 ) ) ;
#11313 = DIRECTION ( 'NONE',  ( -0.01292414190464216336, 1.716839728801787493E-15, -0.9999164797902015955 ) ) ;
#11314 = ORIENTED_EDGE ( 'NONE', *, *, #6858, .T. ) ;
#11315 = CARTESIAN_POINT ( 'NONE',  ( -12.89292530793366431, 186.2522020643850169, 276.6192797974478026 ) ) ;
#11316 = VERTEX_POINT ( 'NONE', #3131 ) ;
#11317 = ORIENTED_EDGE ( 'NONE', *, *, #8498, .F. ) ;
#11318 = DIRECTION ( 'NONE',  ( -0.9999164797902015955, -2.001050586450178695E-22, 0.01292414190464131335 ) ) ;
#11319 = EDGE_CURVE ( 'NONE', #19859, #3243, #13002, .T. ) ;
#11320 = EDGE_CURVE ( 'NONE', #1365, #17586, #7489, .T. ) ;
#11321 = CARTESIAN_POINT ( 'NONE',  ( 26.59130080239608418, 189.4003865961453528, -109.1693451709173956 ) ) ;
#11322 =( LENGTH_UNIT ( ) NAMED_UNIT ( * ) SI_UNIT ( .MILLI., .METRE. ) );
#11323 = DIRECTION ( 'NONE',  ( 0.01292394549866733230, 0.005513023399720419666, 0.9999012842304692006 ) ) ;
#11324 = PLANE ( 'NONE',  #17772 ) ;
#11325 = CARTESIAN_POINT ( 'NONE',  ( -68.43148148480358373, 69.99999999999998579, -86.12277481476654373 ) ) ;
#11326 =( BOUNDED_CURVE ( )  B_SPLINE_CURVE ( 3, ( #22187, #16942, #11759, #20362 ),
 .UNSPECIFIED., .F., .T. ) 
 B_SPLINE_CURVE_WITH_KNOTS ( ( 4, 4 ),
 ( 4.712388980384688786, 5.317223215405117109 ),
 .UNSPECIFIED. ) 
 CURVE ( )  GEOMETRIC_REPRESENTATION_ITEM ( )  RATIONAL_B_SPLINE_CURVE ( ( 1.000000000000000000, 0.9697462613334437709, 0.9697462613334437709, 1.000000000000000000 ) ) 
 REPRESENTATION_ITEM ( '' )  );
#11327 = VERTEX_POINT ( 'NONE', #12553 ) ;
#11328 = CARTESIAN_POINT ( 'NONE',  ( 1.175660927181459158E-14, 45.00000000000000711, 96.00000000000000000 ) ) ;
#11329 = DIRECTION ( 'NONE',  ( 0.000000000000000000, 0.000000000000000000, 1.000000000000000000 ) ) ;
#11330 = CARTESIAN_POINT ( 'NONE',  ( -41.49220022125144425, 173.5884475113861924, 277.1425582878616183 ) ) ;
#11331 = DIRECTION ( 'NONE',  ( 0.000000000000000000, 1.000000000000000000, 0.000000000000000000 ) ) ;
#11332 = EDGE_CURVE ( 'NONE', #10488, #8008, #19203, .T. ) ;
#11333 = CARTESIAN_POINT ( 'NONE',  ( 91.52572433156683473, 77.25800443875652945, -31.39760542763762174 ) ) ;
#11334 = LINE ( 'NONE', #6399, #16267 ) ;
#11335 = VERTEX_POINT ( 'NONE', #8627 ) ;
#11336 = AXIS2_PLACEMENT_3D ( 'NONE', #20322, #8362, #22143 ) ;
#11337 = DIRECTION ( 'NONE',  ( -5.440186201345738641E-18, -1.000000000000000000, -1.334940939666364181E-17 ) ) ;
#11338 = EDGE_CURVE ( 'NONE', #10325, #12065, #12253, .T. ) ;
#11339 = CARTESIAN_POINT ( 'NONE',  ( -41.41899454747574083, 166.0889136240115249, 277.1829612759436827 ) ) ;
#11340 = CARTESIAN_POINT ( 'NONE',  ( -10.83602898747849075, 183.6695850371822019, 308.2317009130024985 ) ) ;
#11341 = AXIS2_PLACEMENT_3D ( 'NONE', #18413, #11400, #2681 ) ;
#11342 = ORIENTED_EDGE ( 'NONE', *, *, #10829, .T. ) ;
#11343 = ORIENTED_EDGE ( 'NONE', *, *, #21564, .T. ) ;
#11344 = DIRECTION ( 'NONE',  ( 2.025474946048326158E-22, -1.000000000000000000, 1.876735158486679638E-22 ) ) ;
#11345 = LINE ( 'NONE', #12849, #11094 ) ;
#11346 = EDGE_CURVE ( 'NONE', #5334, #18942, #3072, .T. ) ;
#11347 = VECTOR ( 'NONE', #16407, 1000.000000000000227 ) ;
#11348 = EDGE_CURVE ( 'NONE', #6325, #12028, #3813, .T. ) ;
#11349 = CARTESIAN_POINT ( 'NONE',  ( -9.065023647928146744, 109.7167603697149474, 130.3064260814875013 ) ) ;
#11350 = CIRCLE ( 'NONE', #3266, 2.000000000000002665 ) ;
#11351 = CARTESIAN_POINT ( 'NONE',  ( -10.82553926660208354, 163.7173592118130045, 130.2889465353590310 ) ) ;
#11352 = ORIENTED_EDGE ( 'NONE', *, *, #15237, .T. ) ;
#11353 = DIRECTION ( 'NONE',  ( 7.125109674161246868E-05, -0.9999848031710253382, 0.005512562950850155054 ) ) ;
#11354 = CARTESIAN_POINT ( 'NONE',  ( -15.42064199597873753, 178.0145423516129881, 312.7841245303434903 ) ) ;
#11355 = ORIENTED_EDGE ( 'NONE', *, *, #14869, .F. ) ;
#11356 = FACE_OUTER_BOUND ( 'NONE', #13576, .T. ) ;
#11357 = LINE ( 'NONE', #8345, #18517 ) ;
#11358 = CARTESIAN_POINT ( 'NONE',  ( -19.00908416305977156, 180.4221386788646271, 76.79453591276953262 ) ) ;
#11359 = DIRECTION ( 'NONE',  ( 0.9999164797902015955, 2.001050586450178695E-22, -0.01292414190464131335 ) ) ;
#11360 = VERTEX_POINT ( 'NONE', #7149 ) ;
#11361 = EDGE_CURVE ( 'NONE', #20680, #22552, #7031, .T. ) ;
#11362 = DIRECTION ( 'NONE',  ( -0.01292394549866741384, -0.005513023399720269613, -0.9999012842304692006 ) ) ;
#11363 = AXIS2_PLACEMENT_3D ( 'NONE', #18396, #8039, #6450 ) ;
#11364 = CIRCLE ( 'NONE', #13572, 10.99999999999999289 ) ;
#11365 = CARTESIAN_POINT ( 'NONE',  ( -5.156377330703347361, 81.19615242270661781, -99.58697729741749072 ) ) ;
#11366 = CIRCLE ( 'NONE', #19426, 3.047499999999988329 ) ;
#11367 = ORIENTED_EDGE ( 'NONE', *, *, #1784, .T. ) ;
#11368 = UNCERTAINTY_MEASURE_WITH_UNIT (LENGTH_MEASURE( 1.000000000000000082E-05 ), #15216, 'distance_accuracy_value', 'NONE');
#11369 = DIRECTION ( 'NONE',  ( -0.9934404589540162256, -0.1135548637187056842, 0.01346653032743081423 ) ) ;
#11370 = CARTESIAN_POINT ( 'NONE',  ( -89.19153677579346606, 89.12515160658807645, 51.27603402924245302 ) ) ;
#11371 = ADVANCED_FACE ( 'NONE', ( #3475 ), #15670, .T. ) ;
#11372 = APPLICATION_PROTOCOL_DEFINITION ( 'draft international standard', 'automotive_design', 1998, #4983 ) ;
#11373 = ORIENTED_EDGE ( 'NONE', *, *, #12494, .T. ) ;
#11374 = DIRECTION ( 'NONE',  ( 0.000000000000000000, 0.000000000000000000, -1.000000000000000000 ) ) ;
#11375 = CARTESIAN_POINT ( 'NONE',  ( -52.78831554946314242, 109.2941709412885700, -43.48738692163240671 ) ) ;
#11376 = ORIENTED_EDGE ( 'NONE', *, *, #14777, .T. ) ;
#11377 = PLANE ( 'NONE',  #19125 ) ;
#11378 = CARTESIAN_POINT ( 'NONE',  ( 1.469576158976823671E-14, 20.00000000000000000, 120.0000000000000000 ) ) ;
#11379 = DIRECTION ( 'NONE',  ( -5.440186201345738641E-18, -1.000000000000000000, -1.334940939666364181E-17 ) ) ;
#11380 = MECHANICAL_DESIGN_GEOMETRIC_PRESENTATION_REPRESENTATION (  '', ( #5127 ), #11744 ) ;
#11381 = DIRECTION ( 'NONE',  ( -0.01292394549866741384, -0.005513023399720269613, -0.9999012842304692006 ) ) ;
#11382 = VERTEX_POINT ( 'NONE', #15784 ) ;
#11383 = FACE_OUTER_BOUND ( 'NONE', #13394, .T. ) ;
#11384 = VERTEX_POINT ( 'NONE', #22614 ) ;
#11385 = DIRECTION ( 'NONE',  ( 0.01292394549866695240, 0.005513023399725255208, 0.9999012842304693116 ) ) ;
#11386 = CARTESIAN_POINT ( 'NONE',  ( -92.63999567227412513, 77.17622496481537553, -28.88303657775555067 ) ) ;
#11387 = PRODUCT_DEFINITION_FORMATION_WITH_SPECIFIED_SOURCE ( 'ANY', '', #8844, .NOT_KNOWN. ) ;
#11388 = CARTESIAN_POINT ( 'NONE',  ( -41.52238611146465530, 166.0448094368136935, 269.1837510020998820 ) ) ;
#11389 = CARTESIAN_POINT ( 'NONE',  ( -38.63026990148117790, 106.6589261331495777, 92.07993625387241821 ) ) ;
#11390 = EDGE_CURVE ( 'NONE', #21389, #21004, #13825, .T. ) ;
#11391 = FACE_OUTER_BOUND ( 'NONE', #1533, .T. ) ;
#11392 =( NAMED_UNIT ( * ) SI_UNIT ( $, .STERADIAN. ) SOLID_ANGLE_UNIT ( ) );
#11393 = AXIS2_PLACEMENT_3D ( 'NONE', #21099, #19601, #21211 ) ;
#11394 = EDGE_CURVE ( 'NONE', #20004, #13491, #13931, .T. ) ;
#11395 = ORIENTED_EDGE ( 'NONE', *, *, #8099, .T. ) ;
#11396 = DIRECTION ( 'NONE',  ( 0.9770372205688160339, -0.2127605332646583802, -0.01145535281434409587 ) ) ;
#11397 = ORIENTED_EDGE ( 'NONE', *, *, #19731, .T. ) ;
#11398 = ORIENTED_EDGE ( 'NONE', *, *, #13633, .T. ) ;
#11399 = CIRCLE ( 'NONE', #11, 2.000000000000001332 ) ;
#11400 = DIRECTION ( 'NONE',  ( 0.01292394549866738782, 0.005513023399720468239, 0.9999012842304692006 ) ) ;
#11401 = TOROIDAL_SURFACE ( 'NONE', #16902, 93.00000000000000000, 2.000000000000000000 ) ;
#11402 = CARTESIAN_POINT ( 'NONE',  ( -90.17340840077037001, 87.01269140057999607, 51.39028561444528975 ) ) ;
#11403 = AXIS2_PLACEMENT_3D ( 'NONE', #8473, #10219, #8158 ) ;
#11404 = VERTEX_POINT ( 'NONE', #1752 ) ;
#11405 = B_SPLINE_CURVE_WITH_KNOTS ( 'NONE', 3,
 ( #111, #3435, #19045, #17348 ),
 .UNSPECIFIED., .F., .F.,
 ( 4, 4 ),
 ( 0.000000000000000000, 0.001461243987307979820 ),
 .UNSPECIFIED. ) ;
#11406 = CARTESIAN_POINT ( 'NONE',  ( -36.80549447617401881, 105.5072037373731888, 92.66220808178287882 ) ) ;
#11407 = CIRCLE ( 'NONE', #3305, 11.00000000000000178 ) ;
#11408 = DIRECTION ( 'NONE',  ( -0.01292394549866695240, -0.005513023399718316314, -0.9999012842304693116 ) ) ;
#11409 = CARTESIAN_POINT ( 'NONE',  ( -70.52438641214237691, 96.69972324582255396, 81.21852732034712119 ) ) ;
#11410 = CARTESIAN_POINT ( 'NONE',  ( -10.79835136690819120, 187.2594016694268646, 276.3428742396645248 ) ) ;
#11411 = CARTESIAN_POINT ( 'NONE',  ( 49.02652807711002936, 169.5865232450209703, -75.63880341251731920 ) ) ;
#11412 = DIRECTION ( 'NONE',  ( 0.01292394549866738782, 0.005513023399720468239, 0.9999012842304692006 ) ) ;
#11413 = PLANE ( 'NONE',  #15214 ) ;
#11414 = VERTEX_POINT ( 'NONE', #10834 ) ;
#11415 = VERTEX_POINT ( 'NONE', #148 ) ;
#11416 = CARTESIAN_POINT ( 'NONE',  ( 51.18466195697779142, 140.5066718483590762, 91.33194389089467791 ) ) ;
#11417 = CARTESIAN_POINT ( 'NONE',  ( -146.5000000000000000, 18.00000000000000355, 8.000000000000015987 ) ) ;
#11418 = CARTESIAN_POINT ( 'NONE',  ( 18.15385362334754404, 184.3839151010789408, 320.8406986940494789 ) ) ;
#11419 = DIRECTION ( 'NONE',  ( 7.125109674161259066E-05, -0.9999848031710252272, 0.005512562950850163727 ) ) ;
#11420 = VECTOR ( 'NONE', #7527, 1000.000000000000000 ) ;
#11421 = CARTESIAN_POINT ( 'NONE',  ( -40.58168163415708563, 127.0293918815982011, 187.3786108412739395 ) ) ;
#11422 =( NAMED_UNIT ( * ) PLANE_ANGLE_UNIT ( ) SI_UNIT ( $, .RADIAN. ) );
#11423 = VECTOR ( 'NONE', #1617, 1000.000000000000114 ) ;
#11424 = AXIS2_PLACEMENT_3D ( 'NONE', #2439, #2324, #16368 ) ;
#11425 = CARTESIAN_POINT ( 'NONE',  ( 1.721625266288826284, 55.00000000000000000, 109.9865264768483968 ) ) ;
#11426 = CONICAL_SURFACE ( 'NONE', #7750, 6.000000000000000888, 0.9599310885968777018 ) ;
#11427 = DIRECTION ( 'NONE',  ( 0.000000000000000000, 0.000000000000000000, -1.000000000000000000 ) ) ;
#11428 = ORIENTED_EDGE ( 'NONE', *, *, #11943, .T. ) ;
#11429 = CARTESIAN_POINT ( 'NONE',  ( 13.04687021101641342, 190.3009381008880609, 320.8498765639175190 ) ) ;
#11430 = ORIENTED_EDGE ( 'NONE', *, *, #18879, .F. ) ;
#11431 = ORIENTED_EDGE ( 'NONE', *, *, #7145, .T. ) ;
#11432 = LINE ( 'NONE', #16736, #17044 ) ;
#11433 = LINE ( 'NONE', #11552, #20345 ) ;
#11434 = ORIENTED_EDGE ( 'NONE', *, *, #8132, .T. ) ;
#11435 = ORIENTED_EDGE ( 'NONE', *, *, #18469, .F. ) ;
#11436 = CIRCLE ( 'NONE', #10692, 4.999999999999990230 ) ;
#11437 = CARTESIAN_POINT ( 'NONE',  ( 75.37956130235376406, 75.02634323965499163, -3.232840821497602768 ) ) ;
#11438 = CARTESIAN_POINT ( 'NONE',  ( 4.169604791867612015, 166.7785703876306513, 322.5944574396354483 ) ) ;
#11439 = AXIS2_PLACEMENT_3D ( 'NONE', #10479, #17491, #16012 ) ;
#11440 = DIRECTION ( 'NONE',  ( 0.09199399308265900077, -0.9957502728239346901, 0.004301093787334665970 ) ) ;
#11441 = DIRECTION ( 'NONE',  ( 8.659560562354942719E-17, -0.7071067811865465735, 0.7071067811865483499 ) ) ;
#11442 = ORIENTED_EDGE ( 'NONE', *, *, #15094, .F. ) ;
#11443 = CARTESIAN_POINT ( 'NONE',  ( -69.07678759757092735, 92.22190598759939917, 85.60612736256487665 ) ) ;
#11444 = DIRECTION ( 'NONE',  ( 1.000000000000000000, 0.000000000000000000, 0.000000000000000000 ) ) ;
#11445 = CARTESIAN_POINT ( 'NONE',  ( -69.96008568250819337, 88.65447058343966091, 68.72499042888327381 ) ) ;
#11446 = LINE ( 'NONE', #11566, #11541 ) ;
#11447 = EDGE_CURVE ( 'NONE', #2088, #11384, #3577, .T. ) ;
#11448 = DIRECTION ( 'NONE',  ( 0.01292394549866740169, 0.005513023399721270548, 0.9999012842304692006 ) ) ;
#11449 = CARTESIAN_POINT ( 'NONE',  ( -9.810751399401715034, 187.6981029871982400, 321.1612345458386812 ) ) ;
#11450 = CARTESIAN_POINT ( 'NONE',  ( 2.830031787867825166, 81.99999999999998579, -80.39798906481894392 ) ) ;
#11451 = VECTOR ( 'NONE', #11359, 1000.000000000000114 ) ;
#11452 = EDGE_CURVE ( 'NONE', #638, #16185, #15561, .T. ) ;
#11453 = CARTESIAN_POINT ( 'NONE',  ( -63.92222308695259869, 94.02752048664899576, 83.80561885825630952 ) ) ;
#11454 = VECTOR ( 'NONE', #20289, 1000.000000000000000 ) ;
#11455 = VECTOR ( 'NONE', #2997, 1000.000000000000227 ) ;
#11456 = VERTEX_POINT ( 'NONE', #20925 ) ;
#11457 = DIRECTION ( 'NONE',  ( 0.9999164797902015955, 2.001050586450178695E-22, -0.01292414190464131335 ) ) ;
#11458 = EDGE_CURVE ( 'NONE', #16242, #2134, #8974, .T. ) ;
#11459 = CARTESIAN_POINT ( 'NONE',  ( -14.65122776820497918, 179.2857995626968943, 310.0431837285613028 ) ) ;
#11460 = ORIENTED_EDGE ( 'NONE', *, *, #3315, .F. ) ;
#11461 = EDGE_LOOP ( 'NONE', ( #4251, #13107, #21103, #12303 ) ) ;
#11462 = AXIS2_PLACEMENT_3D ( 'NONE', #966, #6233, #13259 ) ;
#11463 = CARTESIAN_POINT ( 'NONE',  ( -70.88639693877759385, 71.65513756697318115, -84.11375151051879584 ) ) ;
#11464 = ADVANCED_FACE ( 'NONE', ( #14059 ), #5401, .F. ) ;
#11465 =( BOUNDED_CURVE ( )  B_SPLINE_CURVE ( 3, ( #14372, #19510, #10799, #769 ),
 .UNSPECIFIED., .F., .T. ) 
 B_SPLINE_CURVE_WITH_KNOTS ( ( 4, 4 ),
 ( 5.799006443144739897, 5.835910511159140057 ),
 .UNSPECIFIED. ) 
 CURVE ( )  GEOMETRIC_REPRESENTATION_ITEM ( )  RATIONAL_B_SPLINE_CURVE ( ( 1.000000000000000000, 0.9998865107004337727, 0.9998865107004337727, 1.000000000000000000 ) ) 
 REPRESENTATION_ITEM ( '' )  );
#11466 = AXIS2_PLACEMENT_3D ( 'NONE', #5318, #7585, #14199 ) ;
#11467 = CONICAL_SURFACE ( 'NONE', #19541, 4.999999999999990230, 1.047197551196595855 ) ;
#11468 = CARTESIAN_POINT ( 'NONE',  ( 48.54425533272844717, 166.9503877551599942, 274.0850249888060830 ) ) ;
#11469 = ADVANCED_FACE ( 'NONE', ( #12101 ), #21043, .F. ) ;
#11470 = CARTESIAN_POINT ( 'NONE',  ( 1.364374644014609697E-14, 69.99999999999998579, -9.836443712999143722E-15 ) ) ;
#11471 = ORIENTED_EDGE ( 'NONE', *, *, #5465, .T. ) ;
#11472 = ORIENTED_EDGE ( 'NONE', *, *, #13167, .T. ) ;
#11473 = CARTESIAN_POINT ( 'NONE',  ( 11.91668050545732882, 187.7209081685431613, 304.8819943630518878 ) ) ;
#11474 = CARTESIAN_POINT ( 'NONE',  ( -14.77971672006231252, 178.9662530012681714, 318.9012573015519934 ) ) ;
#11475 = ORIENTED_EDGE ( 'NONE', *, *, #21450, .F. ) ;
#11476 = AXIS2_PLACEMENT_3D ( 'NONE', #4246, #18603, #13230 ) ;
#11477 = ORIENTED_EDGE ( 'NONE', *, *, #3743, .T. ) ;
#11478 = CARTESIAN_POINT ( 'NONE',  ( -7.337194850064199692, 109.6999844229167564, 127.2409188565385421 ) ) ;
#11479 = CARTESIAN_POINT ( 'NONE',  ( -38.92003986412552052, 97.39926864640099780, 83.81297216957182172 ) ) ;
#11480 = DIRECTION ( 'NONE',  ( 0.01292414190464174703, 0.000000000000000000, 0.9999164797902015955 ) ) ;
#11481 = ORIENTED_EDGE ( 'NONE', *, *, #20534, .T. ) ;
#11482 = EDGE_CURVE ( 'NONE', #784, #19287, #12337, .T. ) ;
#11483 =( REPRESENTATION_RELATIONSHIP ('NONE','NONE', #11808, #15770 ) REPRESENTATION_RELATIONSHIP_WITH_TRANSFORMATION ( #17816 )SHAPE_REPRESENTATION_RELATIONSHIP( ) );
#11484 = EDGE_CURVE ( 'NONE', #15391, #15416, #8857, .T. ) ;
#11485 = ORIENTED_EDGE ( 'NONE', *, *, #20850, .F. ) ;
#11486 = CARTESIAN_POINT ( 'NONE',  ( 45.34010913598296355, 168.6466622724117599, 26.02279695137911020 ) ) ;
#11487 = CIRCLE ( 'NONE', #20993, 10.00000000000000355 ) ;
#11488 = ADVANCED_FACE ( 'NONE', ( #13026, #5642 ), #19752, .F. ) ;
#11489 = AXIS2_PLACEMENT_3D ( 'NONE', #22224, #10303, #20745 ) ;
#11490 = CARTESIAN_POINT ( 'NONE',  ( -9.044567292803851188, 186.4032078415717422, 307.5010082646681440 ) ) ;
#11491 = ORIENTED_EDGE ( 'NONE', *, *, #17570, .T. ) ;
#11492 = DIRECTION ( 'NONE',  ( 0.01292394549866738782, 0.005513023399720468239, 0.9999012842304692006 ) ) ;
#11493 = FACE_OUTER_BOUND ( 'NONE', #3320, .T. ) ;
#11494 = ITEM_DEFINED_TRANSFORMATION ( 'NONE', 'NONE', #3365,  #6292 ) ;
#11495 = ORIENTED_EDGE ( 'NONE', *, *, #3822, .T. ) ;
#11496 = CARTESIAN_POINT ( 'NONE',  ( -10.85626963016051150, 114.0998676838791681, 127.2530973345311907 ) ) ;
#11497 = CARTESIAN_POINT ( 'NONE',  ( -49.00853856164501821, 110.7109146754460625, -43.54405268858729983 ) ) ;
#11498 = ADVANCED_FACE ( 'NONE', ( #19648 ), #19988, .T. ) ;
#11499 = ORIENTED_EDGE ( 'NONE', *, *, #13595, .F. ) ;
#11500 = DIRECTION ( 'NONE',  ( 0.9934404589540163366, 0.1135548637187048376, -0.01346653032743036667 ) ) ;
#11501 = DIRECTION ( 'NONE',  ( 1.372099599554306628E-14, -0.000000000000000000, -1.000000000000000000 ) ) ;
#11502 = VECTOR ( 'NONE', #15955, 1000.000000000000227 ) ;
#11503 = CARTESIAN_POINT ( 'NONE',  ( 106.2089377515399065, 72.00000000000000000, 28.62973177816241588 ) ) ;
#11504 = CIRCLE ( 'NONE', #16657, 11.00000000000000178 ) ;
#11505 = CARTESIAN_POINT ( 'NONE',  ( -5.156377330703261208, 81.99999999999998579, -99.58697729741760440 ) ) ;
#11506 = CARTESIAN_POINT ( 'NONE',  ( -44.86761910970069778, 151.3223208568695952, 257.3069776102678929 ) ) ;
#11507 = ORIENTED_EDGE ( 'NONE', *, *, #12026, .F. ) ;
#11508 = CARTESIAN_POINT ( 'NONE',  ( 36.55288090549195346, 94.02752048664900997, -83.45186405039071076 ) ) ;
#11509 = ORIENTED_EDGE ( 'NONE', *, *, #6889, .T. ) ;
#11510 = CARTESIAN_POINT ( 'NONE',  ( -72.65825583664232568, 87.55014249100273105, 69.92630806761130202 ) ) ;
#11511 = CARTESIAN_POINT ( 'NONE',  ( -14.02864438394168722, 325.7329298795136197, 320.4531201330285626 ) ) ;
#11512 = DIRECTION ( 'NONE',  ( 0.9934404589540163366, 0.1135548637187060866, -0.01346653032743036840 ) ) ;
#11513 = DIRECTION ( 'NONE',  ( -7.125109674161259066E-05, 0.9999848031710252272, -0.005512562950850163727 ) ) ;
#11514 = EDGE_CURVE ( 'NONE', #16244, #20892, #17910, .T. ) ;
#11515 = EDGE_LOOP ( 'NONE', ( #5496, #2822 ) ) ;
#11516 = DIRECTION ( 'NONE',  ( -0.01292394549866750231, -0.005513023399722823126, -0.9999012842304692006 ) ) ;
#11517 = VECTOR ( 'NONE', #5025, 999.9999999999998863 ) ;
#11518 = VECTOR ( 'NONE', #14993, 1000.000000000000114 ) ;
#11519 = ORIENTED_EDGE ( 'NONE', *, *, #12293, .F. ) ;
#11520 = CARTESIAN_POINT ( 'NONE',  ( 49.99582398951009310, 170.0000000000008242, -0.6462070952312342076 ) ) ;
#11521 = CARTESIAN_POINT ( 'NONE',  ( -64.99457118636313169, 170.0000000000000284, 0.8400692238016805868 ) ) ;
#11522 = ORIENTED_EDGE ( 'NONE', *, *, #15487, .F. ) ;
#11523 = AXIS2_PLACEMENT_3D ( 'NONE', #19082, #7357, #7245 ) ;
#11524 = AXIS2_PLACEMENT_3D ( 'NONE', #17293, #8223, #12003 ) ;
#11525 = CARTESIAN_POINT ( 'NONE',  ( 1.054933926688728762, 165.4499317482979279, 81.61824794009152129 ) ) ;
#11526 = CARTESIAN_POINT ( 'NONE',  ( -90.17237370337481650, 87.08103440711009569, 51.34890273202512390 ) ) ;
#11527 = EDGE_LOOP ( 'NONE', ( #3110, #7792, #1768, #14768, #2132 ) ) ;
#11528 = EDGE_CURVE ( 'NONE', #719, #309, #11589, .T. ) ;
#11529 = EDGE_CURVE ( 'NONE', #9038, #14045, #15209, .T. ) ;
#11530 = CARTESIAN_POINT ( 'NONE',  ( -41.99649215118849810, 170.0000000000000284, 0.5428139599949243221 ) ) ;
#11531 = DIRECTION ( 'NONE',  ( 0.01292394549866729934, 0.005513023399719703226, 0.9999012842304692006 ) ) ;
#11532 = ORIENTED_EDGE ( 'NONE', *, *, #3743, .F. ) ;
#11533 = AXIS2_PLACEMENT_3D ( 'NONE', #14176, #21153, #5297 ) ;
#11534 = CARTESIAN_POINT ( 'NONE',  ( -49.15102793893406385, 101.1708071963161615, 66.00648395270677327 ) ) ;
#11535 = CARTESIAN_POINT ( 'NONE',  ( -88.17922987063910512, 89.01127821350927150, 51.31456706190138561 ) ) ;
#11536 = CARTESIAN_POINT ( 'NONE',  ( -90.66698955146013361, 79.16774870435553169, 29.00429242512959149 ) ) ;
#11537 = CARTESIAN_POINT ( 'NONE',  ( -37.77863868662843316, 96.04509607205291388, 85.01029411640075750 ) ) ;
#11538 = ORIENTED_EDGE ( 'NONE', *, *, #21490, .F. ) ;
#11539 = DIRECTION ( 'NONE',  ( -7.125109674161246868E-05, 0.9999848031710253382, -0.005512562950850155054 ) ) ;
#11540 = CARTESIAN_POINT ( 'NONE',  ( 20.66604384607886402, 181.9072547581223205, 313.6374335290682893 ) ) ;
#11541 = VECTOR ( 'NONE', #15023, 1000.000000000000000 ) ;
#11542 = CARTESIAN_POINT ( 'NONE',  ( 33.82085273160093664, 93.50464841319750064, -82.93470554904388337 ) ) ;
#11543 = CIRCLE ( 'NONE', #13011, 2.499999999999988010 ) ;
#11544 = DIRECTION ( 'NONE',  ( -1.000000000000000000, 0.000000000000000000, 1.387778780781445676E-14 ) ) ;
#11545 = DIRECTION ( 'NONE',  ( 0.000000000000000000, 0.000000000000000000, 1.000000000000000000 ) ) ;
#11546 = LINE ( 'NONE', #11312, #17303 ) ;
#11547 = CARTESIAN_POINT ( 'NONE',  ( -16.55807878148434753, 175.6145212674599065, 111.6750468525195004 ) ) ;
#11548 = ORIENTED_EDGE ( 'NONE', *, *, #3297, .T. ) ;
#11549 = VECTOR ( 'NONE', #577, 999.9999999999998863 ) ;
#11550 = CARTESIAN_POINT ( 'NONE',  ( -46.77099456471874817, 129.3749911766419700, 250.1451765551053654 ) ) ;
#11551 = ORIENTED_EDGE ( 'NONE', *, *, #14978, .F. ) ;
#11552 = CARTESIAN_POINT ( 'NONE',  ( 65.44129831367571626, 190.1904397277867531, 33.64499135954488196 ) ) ;
#11553 = ORIENTED_EDGE ( 'NONE', *, *, #8238, .T. ) ;
#11554 = AXIS2_PLACEMENT_3D ( 'NONE', #20414, #22240, #17014 ) ;
#11555 = VERTEX_POINT ( 'NONE', #2195 ) ;
#11556 = EDGE_CURVE ( 'NONE', #5939, #14141, #2343, .T. ) ;
#11557 = LINE ( 'NONE', #6386, #19824 ) ;
#11558 = CARTESIAN_POINT ( 'NONE',  ( -50.99096779290750447, 169.5754971982215125, -76.34619179051411209 ) ) ;
#11559 = LINE ( 'NONE', #1446, #3066 ) ;
#11560 = CARTESIAN_POINT ( 'NONE',  ( -10.85626963016051150, 114.0998676838791681, 127.2530973345311907 ) ) ;
#11561 = CARTESIAN_POINT ( 'NONE',  ( -66.42677970909001317, 189.3893605493459233, -109.9672025422466959 ) ) ;
#11562 = CYLINDRICAL_SURFACE ( 'NONE', #2564, 2.499999999999988010 ) ;
#11563 = CARTESIAN_POINT ( 'NONE',  ( 153.9999999999992610, 18.00000000000000355, 53.76161406891468175 ) ) ;
#11564 = CIRCLE ( 'NONE', #1662, 10.00000000000005862 ) ;
#11565 = CARTESIAN_POINT ( 'NONE',  ( -41.52238611146507452, 166.0448094368137504, 269.1837510020998820 ) ) ;
#11566 = CARTESIAN_POINT ( 'NONE',  ( 163.9999999999998863, 18.00000000000000355, -8.000000000002268408 ) ) ;
#11567 = CARTESIAN_POINT ( 'NONE',  ( 92.46788464407295294, 79.04398536104956463, -28.62013883513311896 ) ) ;
#11568 = CARTESIAN_POINT ( 'NONE',  ( -8.676042597691862923, 185.9097051440071766, 321.2330616462555781 ) ) ;
#11569 = CARTESIAN_POINT ( 'NONE',  ( 92.79593043952061748, 70.16589065052625074, 59.06731773122648832 ) ) ;
#11570 = CARTESIAN_POINT ( 'NONE',  ( 49.56856857351093737, 189.4900557983233398, -93.20024246017386815 ) ) ;
#11571 = PRODUCT_RELATED_PRODUCT_CATEGORY ( 'part', '', ( #8081 ) ) ;
#11572 = ORIENTED_EDGE ( 'NONE', *, *, #21604, .F. ) ;
#11573 = DIRECTION ( 'NONE',  ( -2.025474946048326158E-22, 1.000000000000000000, -1.876735158486679638E-22 ) ) ;
#11574 = CARTESIAN_POINT ( 'NONE',  ( -13.87886915313458580, 180.3914499437145764, 310.5935113253086683 ) ) ;
#11575 = ORIENTED_EDGE ( 'NONE', *, *, #7680, .F. ) ;
#11576 = B_SPLINE_CURVE_WITH_KNOTS ( 'NONE', 3,
 ( #5361, #17115, #8355, #15399, #22346, #6643 ),
 .UNSPECIFIED., .F., .F.,
 ( 4, 2, 4 ),
 ( 2.380730969743839749E-07, 0.002629065763328481461, 0.005257893453559988640 ),
 .UNSPECIFIED. ) ;
#11577 = ORIENTED_EDGE ( 'NONE', *, *, #17648, .F. ) ;
#11578 = VECTOR ( 'NONE', #21350, 1000.000000000000114 ) ;
#11579 = PRODUCT_DEFINITION_SHAPE ( 'NONE', 'NONE',  #15651 ) ;
#11580 = DIRECTION ( 'NONE',  ( -0.01292414190464137060, 0.000000000000000000, -0.9999164797902015955 ) ) ;
#11581 = EDGE_CURVE ( 'NONE', #19957, #5442, #18711, .T. ) ;
#11582 = ORIENTED_EDGE ( 'NONE', *, *, #10855, .F. ) ;
#11583 = LINE ( 'NONE', #2840, #14074 ) ;
#11584 = CARTESIAN_POINT ( 'NONE',  ( 3.872354045398203937, 166.6517708494369856, 299.5967279023338392 ) ) ;
#11585 = LINE ( 'NONE', #793, #5117 ) ;
#11586 = EDGE_LOOP ( 'NONE', ( #11635, #22125, #4276, #14670, #10410 ) ) ;
#11587 = ORIENTED_EDGE ( 'NONE', *, *, #5139, .F. ) ;
#11588 = CARTESIAN_POINT ( 'NONE',  ( 11.82412558468182873, 187.7865448877315657, 307.7681344816915612 ) ) ;
#11589 = B_SPLINE_CURVE_WITH_KNOTS ( 'NONE', 3,
 ( #714, #18400, #18287, #11166, #11051, #2322, #16366, #14408, #604, #14521, #12899, #7709, #21372, #2437, #21583, #5989 ),
 .UNSPECIFIED., .F., .F.,
 ( 4, 2, 2, 2, 2, 2, 2, 4 ),
 ( 0.000000000000000000, 0.0003976838443733619953, 0.0007953676887467239906, 0.001193051533120085932, 0.001590735377493447981, 0.002386103066240156251, 0.002783786910613529793, 0.003181470754986902901 ),
 .UNSPECIFIED. ) ;
#11590 = CARTESIAN_POINT ( 'NONE',  ( -55.30663963734144772, 126.9329139721032931, 170.0677384248578790 ) ) ;
#11591 = CARTESIAN_POINT ( 'NONE',  ( -106.2142196127746558, 77.44923501812726840, -28.61015647369513459 ) ) ;
#11592 = DIRECTION ( 'NONE',  ( -0.01292394549866745720, -0.005513023399720816918, -0.9999012842304692006 ) ) ;
#11593 = AXIS2_PLACEMENT_3D ( 'NONE', #5636, #12672, #12892 ) ;
#11594 = CARTESIAN_POINT ( 'NONE',  ( 59.61792454239376582, 143.9050905090123820, 163.4882421145072726 ) ) ;
#11595 = ORIENTED_EDGE ( 'NONE', *, *, #5276, .F. ) ;
#11596 = ADVANCED_FACE ( 'NONE', ( #7832 ), #9426, .T. ) ;
#11597 = CARTESIAN_POINT ( 'NONE',  ( 81.70668847916368804, 104.4142135623730780, -73.64792636435126383 ) ) ;
#11598 = CARTESIAN_POINT ( 'NONE',  ( 20.04096596137404873, 146.7968166218097110, 276.4111418983213184 ) ) ;
#11599 = CARTESIAN_POINT ( 'NONE',  ( 146.4999999999998863, 18.00000000000000355, 8.000000000001989520 ) ) ;
#11600 = EDGE_CURVE ( 'NONE', #16835, #21699, #7363, .T. ) ;
#11601 = EDGE_LOOP ( 'NONE', ( #17356, #15255, #2334, #8190 ) ) ;
#11602 = CARTESIAN_POINT ( 'NONE',  ( -34.77171180284935303, 125.3750519639578727, 250.0121371040530676 ) ) ;
#11603 = DIRECTION ( 'NONE',  ( 7.125109674160258889E-05, -0.9999848031710252272, 0.005512562950849897447 ) ) ;
#11604 = EDGE_CURVE ( 'NONE', #16244, #3397, #16327, .T. ) ;
#11606 = ORIENTED_EDGE ( 'NONE', *, *, #12588, .T. ) ;
#11605 = EDGE_LOOP ( 'NONE', ( #690, #19662, #11237, #1462 ) ) ;
#11607 = EDGE_CURVE ( 'NONE', #16346, #16446, #13379, .T. ) ;
#11608 = DIRECTION ( 'NONE',  ( 0.9999164797902015955, 6.965998958219364448E-18, -0.01292414190464157182 ) ) ;
#11609 = EDGE_CURVE ( 'NONE', #10751, #9211, #8935, .T. ) ;
#11610 = CARTESIAN_POINT ( 'NONE',  ( -50.60905219909545849, 112.8337759852537090, -43.53507023493251893 ) ) ;
#11611 = VERTEX_POINT ( 'NONE', #6340 ) ;
#11612 = CARTESIAN_POINT ( 'NONE',  ( 89.66113247980437961, 100.6041916471017856, 63.72504470331089266 ) ) ;
#11613 = LINE ( 'NONE', #15068, #12206 ) ;
#11614 = DIRECTION ( 'NONE',  ( -0.9232306267972774094, -1.069144893909151832E-19, 0.3842462878721230046 ) ) ;
#11615 = LINE ( 'NONE', #3196, #5368 ) ;
#11616 = DIRECTION ( 'NONE',  ( -0.9770372205688155898, 0.2127605332646606839, 0.01145535281434407679 ) ) ;
#11617 = ORIENTED_EDGE ( 'NONE', *, *, #1716, .F. ) ;
#11618 = CARTESIAN_POINT ( 'NONE',  ( -66.71891079484507259, 98.29072687177919931, 79.57820418736568513 ) ) ;
#11619 = VERTEX_POINT ( 'NONE', #18841 ) ;
#11620 = CARTESIAN_POINT ( 'NONE',  ( -72.65963751957909267, 87.42236182341126494, 69.77244766351077487 ) ) ;
#11621 = DIRECTION ( 'NONE',  ( -0.01292414190464130641, 0.000000000000000000, -0.9999164797902015955 ) ) ;
#11622 = CARTESIAN_POINT ( 'NONE',  ( -41.88967587883006871, 162.6016759231961260, 277.2082720574355790 ) ) ;
#11623 = CARTESIAN_POINT ( 'NONE',  ( 0.000000000000000000, 37.00000000000000711, 0.000000000000000000 ) ) ;
#11624 = ADVANCED_FACE ( 'NONE', ( #1295 ), #17030, .F. ) ;
#11625 = DIRECTION ( 'NONE',  ( 1.372099599554306628E-14, -0.000000000000000000, -1.000000000000000000 ) ) ;
#11626 = CARTESIAN_POINT ( 'NONE',  ( 53.22065341430143803, 129.3749911766419700, 248.8527623646411939 ) ) ;
#11627 = EDGE_LOOP ( 'NONE', ( #18850, #11209, #5745, #16009 ) ) ;
#11628 = DIRECTION ( 'NONE',  ( -0.9999164797902020396, 2.081668151161667201E-14, 0.01292414190462050187 ) ) ;
#11629 = EDGE_CURVE ( 'NONE', #3254, #6576, #18722, .T. ) ;
#11630 = DIRECTION ( 'NONE',  ( -7.125109674118361251E-05, 0.9999848031710253382, -0.005512562950849477644 ) ) ;
#11631 = VERTEX_POINT ( 'NONE', #22260 ) ;
#11632 = DIRECTION ( 'NONE',  ( -7.125109674381882011E-05, 0.9999848031710253382, -0.005512562950849702291 ) ) ;
#11633 = CARTESIAN_POINT ( 'NONE',  ( -90.12935778220864336, 87.38120584935140300, 51.16641606481163507 ) ) ;
#11634 = CARTESIAN_POINT ( 'NONE',  ( 40.65822637310715493, 91.17157287525387233, 84.25167897319539634 ) ) ;
#11635 = ORIENTED_EDGE ( 'NONE', *, *, #22511, .T. ) ;
#11636 = EDGE_CURVE ( 'NONE', #14619, #21224, #4447, .T. ) ;
#11637 = DIRECTION ( 'NONE',  ( -7.125109674156763692E-05, 0.9999848031710254492, -0.005512562950846685607 ) ) ;
#11638 = FACE_BOUND ( 'NONE', #19085, .T. ) ;
#11639 = LINE ( 'NONE', #22177, #16486 ) ;
#11640 = DIRECTION ( 'NONE',  ( -0.01292394549866704608, -0.005513023399718946886, -0.9999012842304692006 ) ) ;
#11641 = CARTESIAN_POINT ( 'NONE',  ( 2.067862704742617463, 69.99999999999998579, 159.9866367664322979 ) ) ;
#11642 = DIRECTION ( 'NONE',  ( 0.9999164797902015955, 6.965998958219364448E-18, -0.01292414190464157182 ) ) ;
#11643 = CARTESIAN_POINT ( 'NONE',  ( -51.28019763314280510, 189.4953702477336890, -90.93270303136451105 ) ) ;
#11644 = ORIENTED_EDGE ( 'NONE', *, *, #17041, .F. ) ;
#11645 = AXIS2_PLACEMENT_3D ( 'NONE', #16901, #1169, #15072 ) ;
#11646 = CARTESIAN_POINT ( 'NONE',  ( -64.99457118636313169, 170.0000000000000284, 0.8400692238016805868 ) ) ;
#11647 = DIRECTION ( 'NONE',  ( 7.125109674364534776E-05, -0.9999848031710252272, 0.005512562950849704893 ) ) ;
#11648 = CARTESIAN_POINT ( 'NONE',  ( 89.99335928417747255, 79.29537036754122425, -29.40900737050180780 ) ) ;
#11649 = CARTESIAN_POINT ( 'NONE',  ( -59.86179714464044821, 114.2071845241163999, 165.4942746823298023 ) ) ;
#11650 = CARTESIAN_POINT ( 'NONE',  ( -8.661992976619229623, 145.5753956220379166, 277.8423689545541038 ) ) ;
#11651 = ORIENTED_EDGE ( 'NONE', *, *, #247, .F. ) ;
#11652 =( NAMED_UNIT ( * ) PLANE_ANGLE_UNIT ( ) SI_UNIT ( $, .RADIAN. ) );
#11653 = EDGE_CURVE ( 'NONE', #19436, #8712, #8042, .T. ) ;
#11654 = DIRECTION ( 'NONE',  ( 0.9999164797902015955, 6.965998958219364448E-18, -0.01292414190464157182 ) ) ;
#11655 = LINE ( 'NONE', #16952, #4087 ) ;
#11656 = VERTEX_POINT ( 'NONE', #4930 ) ;
#11657 = CARTESIAN_POINT ( 'NONE',  ( -13.08489379702671052, 184.1207951144569961, 278.6477083146653513 ) ) ;
#11658 = VERTEX_POINT ( 'NONE', #15419 ) ;
#11659 = ORIENTED_EDGE ( 'NONE', *, *, #13656, .F. ) ;
#11660 = TOROIDAL_SURFACE ( 'NONE', #7612, 77.00000000000002842, 2.000000000000000000 ) ;
#11661 = PLANE ( 'NONE',  #18156 ) ;
#11662 = ORIENTED_EDGE ( 'NONE', *, *, #2912, .F. ) ;
#11663 = EDGE_CURVE ( 'NONE', #7781, #12967, #11298, .T. ) ;
#11664 = CARTESIAN_POINT ( 'NONE',  ( -49.49165101955345136, 107.3307887671683432, 70.99333137697747986 ) ) ;
#11665 = CARTESIAN_POINT ( 'NONE',  ( -55.33980451424918101, 138.9189490516561136, 167.5018344588715138 ) ) ;
#11666 = CARTESIAN_POINT ( 'NONE',  ( -109.7386064778677621, 75.43227853978193309, -7.937952133666764887 ) ) ;
#11667 = DIRECTION ( 'NONE',  ( 0.000000000000000000, -1.000000000000000000, 0.000000000000000000 ) ) ;
#11668 = DIRECTION ( 'NONE',  ( -0.9934404589540162256, -0.1135548637187060589, 0.01346653032743275885 ) ) ;
#11669 = CARTESIAN_POINT ( 'NONE',  ( 17.01736581203620702, 186.7717766984534080, 276.5372814302687061 ) ) ;
#11670 = ORIENTED_EDGE ( 'NONE', *, *, #13322, .F. ) ;
#11671 = DIRECTION ( 'NONE',  ( 0.01292414190464523903, 0.000000000000000000, 0.9999164797902017066 ) ) ;
#11672 = DIRECTION ( 'NONE',  ( 0.9999164797902017066, 6.965998958219365988E-18, -0.01292414190464157356 ) ) ;
#11673 = LINE ( 'NONE', #5087, #17764 ) ;
#11674 = CARTESIAN_POINT ( 'NONE',  ( -66.42677970909001317, 189.3893605493459233, -109.9672025422466959 ) ) ;
#11675 = CARTESIAN_POINT ( 'NONE',  ( -56.88925295215435085, 118.2576901802692646, 47.62393161023230448 ) ) ;
#11676 = VERTEX_POINT ( 'NONE', #16798 ) ;
#11677 = DIRECTION ( 'NONE',  ( 0.01292394549866734098, 0.005513023399720419666, 0.9999012842304692006 ) ) ;
#11678 = ORIENTED_EDGE ( 'NONE', *, *, #12739, .T. ) ;
#11679 = ORIENTED_EDGE ( 'NONE', *, *, #12460, .F. ) ;
#11680 = EDGE_CURVE ( 'NONE', #12459, #21648, #15202, .T. ) ;
#11681 = CYLINDRICAL_SURFACE ( 'NONE', #11756, 4.200000000000005507 ) ;
#11682 = CARTESIAN_POINT ( 'NONE',  ( -8.449107425469586374, 185.4541341740502958, 308.0383059716917273 ) ) ;
#11683 = EDGE_CURVE ( 'NONE', #2811, #10705, #8169, .T. ) ;
#11684 = ORIENTED_EDGE ( 'NONE', *, *, #2286, .F. ) ;
#11685 = CARTESIAN_POINT ( 'NONE',  ( 6.254127940454620393, 70.00000000000000000, -84.87602797277139643 ) ) ;
#11686 = CONICAL_SURFACE ( 'NONE', #17925, 3.399999999999991918, 1.029744258676652313 ) ;
#11687 = EDGE_LOOP ( 'NONE', ( #16796, #7240 ) ) ;
#11688 = CARTESIAN_POINT ( 'NONE',  ( 90.02055463237803679, 95.44063823554751025, -63.21629334023821656 ) ) ;
#11689 = CYLINDRICAL_SURFACE ( 'NONE', #15178, 4.500000000000006217 ) ;
#11690 = CARTESIAN_POINT ( 'NONE',  ( 17.39319413858549268, 146.5330681163042073, 276.7522768435346165 ) ) ;
#11691 = DIRECTION ( 'NONE',  ( -0.7944560844389304544, 0.000000000000000000, -0.6073216033519334145 ) ) ;
#11692 = VECTOR ( 'NONE', #1072, 1000.000000000000227 ) ;
#11693 = CARTESIAN_POINT ( 'NONE',  ( 1.028703311283776507E-14, 37.00000000000000711, 83.99999999999998579 ) ) ;
#11694 = DIRECTION ( 'NONE',  ( 0.9934404589540163366, 0.1135548637187051429, -0.01346653032743023309 ) ) ;
#11695 = PRESENTATION_LAYER_ASSIGNMENT (  '', '', ( #10238 ) ) ;
#11696 = CARTESIAN_POINT ( 'NONE',  ( -37.16795793340686060, 95.89798883583556233, 85.13463587459933990 ) ) ;
#11697 = CARTESIAN_POINT ( 'NONE',  ( -89.66113247980429435, 100.6041916471018709, -63.72504470331098503 ) ) ;
#11698 = ORIENTED_EDGE ( 'NONE', *, *, #18655, .F. ) ;
#11699 = DIRECTION ( 'NONE',  ( -0.006350819331214699499, 0.8709385446395367936, -0.4913509118287948674 ) ) ;
#11700 = ORIENTED_EDGE ( 'NONE', *, *, #9823, .T. ) ;
#11701 = PLANE ( 'NONE',  #13071 ) ;
#11702 = CARTESIAN_POINT ( 'NONE',  ( -11.19153202869804353, 137.5572120012638777, 101.3144779797563189 ) ) ;
#11703 = CARTESIAN_POINT ( 'NONE',  ( -109.3552458118615363, 88.71869973106718987, 50.59427279859775695 ) ) ;
#11704 = CARTESIAN_POINT ( 'NONE',  ( -27.84085044979666179, 324.1152701834824938, 311.0106090768176159 ) ) ;
#11705 = TOROIDAL_SURFACE ( 'NONE', #12458, 97.00000000000004263, 2.000000000000000000 ) ;
#11706 = B_SPLINE_CURVE_WITH_KNOTS ( 'NONE', 3,
 ( #5483, #14595, #21452, #19392, #1825, #5712, #5605, #17820, #12744, #21550, #17924, #21223, #8938, #14246 ),
 .UNSPECIFIED., .F., .F.,
 ( 4, 2, 2, 2, 2, 2, 4 ),
 ( 0.000000000000000000, 0.001153947729383741775, 0.002307895458767483549, 0.002884869323459376012, 0.003461843188151268041, 0.004038817052843160504, 0.004615790917535052967 ),
 .UNSPECIFIED. ) ;
#11707 = DIRECTION ( 'NONE',  ( -0.4540042784513456109, 0.000000000000000000, 0.8909995034498464639 ) ) ;
#11708 = CARTESIAN_POINT ( 'NONE',  ( 48.49599547156344670, 174.4605628858501802, 275.9746324660413279 ) ) ;
#11709 = APPLICATION_PROTOCOL_DEFINITION ( 'draft international standard', 'automotive_design', 1998, #17627 ) ;
#11710 = VECTOR ( 'NONE', #10549, 1000.000000000000000 ) ;
#11711 = ORIENTED_EDGE ( 'NONE', *, *, #10512, .T. ) ;
#11712 = EDGE_CURVE ( 'NONE', #16304, #18095, #6663, .T. ) ;
#11713 = CARTESIAN_POINT ( 'NONE',  ( 38.89810712971355855, 91.17157287525387233, -85.50986645835283184 ) ) ;
#11714 = LINE ( 'NONE', #18708, #20285 ) ;
#11715 = DIRECTION ( 'NONE',  ( -0.9999164797902017066, -7.033761593999711556E-18, 0.01292414190464155968 ) ) ;
#11716 = CYLINDRICAL_SURFACE ( 'NONE', #16992, 6.250000000000000000 ) ;
#11717 = CARTESIAN_POINT ( 'NONE',  ( 49.99895903776670991, 126.0006686604749291, -0.4036543253946939802 ) ) ;
#11718 = DIRECTION ( 'NONE',  ( -0.004829518060344428765, -0.03945926991566312686, -0.9992095084480668854 ) ) ;
#11719 = FACE_OUTER_BOUND ( 'NONE', #9091, .T. ) ;
#11720 = VERTEX_POINT ( 'NONE', #22158 ) ;
#11721 = CARTESIAN_POINT ( 'NONE',  ( -54.52327687265815825, 0.000000000000000000, -111.3697098814011923 ) ) ;
#11722 = CARTESIAN_POINT ( 'NONE',  ( 14.23917046504717021, 105.7413430127404439, 134.4755589474307840 ) ) ;
#11723 = ORIENTED_EDGE ( 'NONE', *, *, #21545, .F. ) ;
#11724 = FACE_OUTER_BOUND ( 'NONE', #19098, .T. ) ;
#11725 = DIRECTION ( 'NONE',  ( 0.000000000000000000, 0.000000000000000000, -1.000000000000000000 ) ) ;
#11726 = CARTESIAN_POINT ( 'NONE',  ( 105.9930786687657616, 70.38870405239202910, 29.41946405304832268 ) ) ;
#11727 = LINE ( 'NONE', #10231, #12487 ) ;
#11728 = AXIS2_PLACEMENT_3D ( 'NONE', #2192, #16363, #5518 ) ;
#11729 = STYLED_ITEM ( 'NONE', ( #19198 ), #17376 ) ;
#11730 = ORIENTED_EDGE ( 'NONE', *, *, #22245, .F. ) ;
#11731 = CARTESIAN_POINT ( 'NONE',  ( -18.87984470807310089, 180.4772689128618310, 86.79354875507422662 ) ) ;
#11732 = DIRECTION ( 'NONE',  ( 7.125109674403837105E-05, -0.9999848031710252272, 0.005512562950847867821 ) ) ;
#11733 = AXIS2_PLACEMENT_3D ( 'NONE', #96, #3765, #2043 ) ;
#11734 = EDGE_CURVE ( 'NONE', #22035, #17658, #1396, .T. ) ;
#11735 = EDGE_LOOP ( 'NONE', ( #4346, #21722, #10566, #13372 ) ) ;
#11736 = CARTESIAN_POINT ( 'NONE',  ( 39.18801548568782067, 107.5071733437152375, 91.66894817112843441 ) ) ;
#11737 = ADVANCED_FACE ( 'NONE', ( #2667 ), #7936, .F. ) ;
#11738 = FACE_OUTER_BOUND ( 'NONE', #17972, .T. ) ;
#11739 = EDGE_LOOP ( 'NONE', ( #13663, #20229, #16813, #21782, #5954 ) ) ;
#11740 = CARTESIAN_POINT ( 'NONE',  ( -90.14075885923632825, 87.33211882309382190, 51.19633987193193292 ) ) ;
#11741 = AXIS2_PLACEMENT_3D ( 'NONE', #9671, #13357, #946 ) ;
#11743 = EDGE_LOOP ( 'NONE', ( #11572, #8580, #8872, #9334 ) ) ;
#11742 = VERTEX_POINT ( 'NONE', #6213 ) ;
#11744 =( GEOMETRIC_REPRESENTATION_CONTEXT ( 3 ) GLOBAL_UNCERTAINTY_ASSIGNED_CONTEXT ( ( #9764 ) ) GLOBAL_UNIT_ASSIGNED_CONTEXT ( ( #15931, #8755, #14894 ) ) REPRESENTATION_CONTEXT ( 'NONE', 'WORKASPACE' ) );
#11745 = EDGE_CURVE ( 'NONE', #15608, #5658, #18138, .T. ) ;
#11746 = CARTESIAN_POINT ( 'NONE',  ( 0.000000000000000000, 25.00000000000000000, 0.000000000000000000 ) ) ;
#11747 = EDGE_CURVE ( 'NONE', #5484, #5811, #11150, .T. ) ;
#11748 = DIRECTION ( 'NONE',  ( 7.125109674364534776E-05, -0.9999848031710252272, 0.005512562950849704893 ) ) ;
#11749 = CARTESIAN_POINT ( 'NONE',  ( 1.054933926688728762, 165.4499317482979279, 81.61824794009152129 ) ) ;
#11750 = ORIENTED_EDGE ( 'NONE', *, *, #2786, .T. ) ;
#11751 = CARTESIAN_POINT ( 'NONE',  ( -12.64660359835458792, 105.6831695174542745, 124.2703293933457758 ) ) ;
#11752 = CARTESIAN_POINT ( 'NONE',  ( -88.16874431701178594, 88.69758567471752997, 52.43331850404257466 ) ) ;
#11753 = CARTESIAN_POINT ( 'NONE',  ( -51.99565694909051672, 170.0000000000000284, 0.6720553790413400508 ) ) ;
#11754 = CARTESIAN_POINT ( 'NONE',  ( -70.93357090261923759, 91.46354453597339784, -84.07396062241134871 ) ) ;
#11755 = EDGE_CURVE ( 'NONE', #9279, #7202, #21411, .T. ) ;
#11756 = AXIS2_PLACEMENT_3D ( 'NONE', #11339, #14931, #4545 ) ;
#11757 = ORIENTED_EDGE ( 'NONE', *, *, #7786, .F. ) ;
#11758 = CARTESIAN_POINT ( 'NONE',  ( -92.40872671617950118, 72.00000000000000000, 33.19707612406966746 ) ) ;
#11759 = CARTESIAN_POINT ( 'NONE',  ( -88.28334709335607045, 71.38106462369736960, 62.47119547224009040 ) ) ;
#11760 = CARTESIAN_POINT ( 'NONE',  ( 89.41602473586598876, 79.46258270018843461, -29.93333348547120210 ) ) ;
#11761 = FACE_OUTER_BOUND ( 'NONE', #7670, .T. ) ;
#11762 = CARTESIAN_POINT ( 'NONE',  ( -12.87580311257307031, 148.6428581928619792, 277.0426180699594738 ) ) ;
#11763 = ORIENTED_EDGE ( 'NONE', *, *, #3162, .F. ) ;
#11764 = DIRECTION ( 'NONE',  ( 0.000000000000000000, 1.000000000000000000, 0.000000000000000000 ) ) ;
#11765 = AXIS2_PLACEMENT_3D ( 'NONE', #774, #18235, #11448 ) ;
#11766 = ADVANCED_FACE ( 'NONE', ( #18944 ), #15645, .F. ) ;
#11767 = TOROIDAL_SURFACE ( 'NONE', #14721, 8.000000000000014211, 2.000000000000000000 ) ;
#11768 = EDGE_CURVE ( 'NONE', #10450, #17005, #20880, .T. ) ;
#11769 = AXIS2_PLACEMENT_3D ( 'NONE', #7250, #17740, #21371 ) ;
#11770 = CARTESIAN_POINT ( 'NONE',  ( -64.03197570747913403, 99.62212517233105302, 75.31426563926737572 ) ) ;
#11771 = ORIENTED_EDGE ( 'NONE', *, *, #3086, .F. ) ;
#11772 = AXIS2_PLACEMENT_3D ( 'NONE', #19690, #11223, #16641 ) ;
#11773 = CARTESIAN_POINT ( 'NONE',  ( -8.806159735684131462, 187.4460332972412857, 276.6223298942460360 ) ) ;
#11774 = ORIENTED_EDGE ( 'NONE', *, *, #12999, .F. ) ;
#11775 = ADVANCED_FACE ( 'NONE', ( #21230 ), #1618, .F. ) ;
#11776 = CARTESIAN_POINT ( 'NONE',  ( -21.61166911467453389, 64.93155780410928912, -124.5625524242976070 ) ) ;
#11777 = VECTOR ( 'NONE', #11457, 1000.000000000000114 ) ;
#11779 = EDGE_LOOP ( 'NONE', ( #14099, #3004, #15909 ) ) ;
#11778 = VERTEX_POINT ( 'NONE', #17477 ) ;
#11780 = SURFACE_STYLE_FILL_AREA ( #4741 ) ;
#11781 = DIRECTION ( 'NONE',  ( 0.01292414190464131508, 0.000000000000000000, 0.9999164797902017066 ) ) ;
#11782 = EDGE_CURVE ( 'NONE', #10176, #7226, #7126, .T. ) ;
#11783 = VECTOR ( 'NONE', #1371, 999.9999999999998863 ) ;
#11784 = CARTESIAN_POINT ( 'NONE',  ( -88.16157026904451754, 88.04290212818517602, 53.06700061362226961 ) ) ;
#11785 = AXIS2_PLACEMENT_3D ( 'NONE', #21187, #7406, #5672 ) ;
#11786 = B_SPLINE_CURVE_WITH_KNOTS ( 'NONE', 3,
 ( #21784, #16223, #6075, #3991, #12862, #18366, #7574, #19841, #7461, #16340, #12993, #11254, #13104, #14499, #21460, #18045 ),
 .UNSPECIFIED., .F., .F.,
 ( 4, 2, 2, 2, 2, 2, 2, 4 ),
 ( 6.938893903907228378E-18, 0.0004210512469646337250, 0.0008421024939292605111, 0.001684204987858477871, 0.002105256234823093056, 0.002526307481787708024, 0.002947358728752323426, 0.003368409975716938395 ),
 .UNSPECIFIED. ) ;
#11787 = CARTESIAN_POINT ( 'NONE',  ( -92.89382307712746467, 70.12557134413805215, -58.91325363510486568 ) ) ;
#11788 = EDGE_CURVE ( 'NONE', #2512, #16435, #1832, .T. ) ;
#11789 = CARTESIAN_POINT ( 'NONE',  ( 16.54955802965976730, 187.9265162623472349, 275.8329542685239630 ) ) ;
#11790 = DIRECTION ( 'NONE',  ( 7.125109674403837105E-05, -0.9999848031710252272, 0.005512562950847867821 ) ) ;
#11791 = LINE ( 'NONE', #15476, #36 ) ;
#11792 = PLANE ( 'NONE',  #21743 ) ;
#11793 = DIRECTION ( 'NONE',  ( 0.01292394549866738608, 0.005513023399720699824, 0.9999012842304692006 ) ) ;
#11794 = CARTESIAN_POINT ( 'NONE',  ( 90.65403358069686135, 80.14440291447091624, -32.01641220276457034 ) ) ;
#11795 = VERTEX_POINT ( 'NONE', #4042 ) ;
#11796 = CIRCLE ( 'NONE', #14749, 95.00000000000001421 ) ;
#11797 = DIRECTION ( 'NONE',  ( 0.9999164797902015955, 2.001050586450176109E-22, -0.01292414190464270113 ) ) ;
#11798 = ORIENTED_EDGE ( 'NONE', *, *, #12048, .T. ) ;
#11799 = EDGE_CURVE ( 'NONE', #18358, #17537, #15707, .T. ) ;
#11800 = ORIENTED_EDGE ( 'NONE', *, *, #17285, .F. ) ;
#11801 = LINE ( 'NONE', #3057, #4770 ) ;
#11802 = DIRECTION ( 'NONE',  ( 7.125109674160325297E-05, -0.9999848031710252272, 0.005512562950849327591 ) ) ;
#11803 = ORIENTED_EDGE ( 'NONE', *, *, #9562, .T. ) ;
#11804 = CARTESIAN_POINT ( 'NONE',  ( -6.157660283484229780, 188.8249578887279085, 276.4363886600518185 ) ) ;
#11805 = EDGE_LOOP ( 'NONE', ( #2615, #9844, #18063, #3189 ) ) ;
#11806 = AXIS2_PLACEMENT_3D ( 'NONE', #10237, #4937, #13699 ) ;
#11807 =( GEOMETRIC_REPRESENTATION_CONTEXT ( 3 ) GLOBAL_UNCERTAINTY_ASSIGNED_CONTEXT ( ( #1666 ) ) GLOBAL_UNIT_ASSIGNED_CONTEXT ( ( #7282, #3392, #287 ) ) REPRESENTATION_CONTEXT ( 'NONE', 'WORKASPACE' ) );
#11808 = SHAPE_REPRESENTATION ( 'MAS-425', ( #8088, #20961, #8845, #3365, #16233, #15133, #9227, #4400, #21637, #15817, #3680, #5886, #10290, #21995, #17651, #1132, #7341, #11772, #10662, #1486, #386, #13613, #18723, #19079, #18, #18349, #7729, #6253, #2585, #12869, #13591, #2945, #22345, #12128, #6606, #3668, #18012 ), #16539 ) ;
#11809 = AXIS2_PLACEMENT_3D ( 'NONE', #20097, #11513, #18076 ) ;
#11810 = CARTESIAN_POINT ( 'NONE',  ( -68.68766895589030241, 71.65104882840749667, 85.91861595181278233 ) ) ;
#11811 = AXIS2_PLACEMENT_3D ( 'NONE', #900, #4426, #16856 ) ;
#11812 = ORIENTED_EDGE ( 'NONE', *, *, #11788, .T. ) ;
#11813 = DIRECTION ( 'NONE',  ( 0.006350819331212799977, -0.8709385446395345731, 0.4913509118287983091 ) ) ;
#11814 = DIRECTION ( 'NONE',  ( -5.440186201345785633E-18, -1.000000000000000000, -1.334940939666367878E-17 ) ) ;
#11815 = FACE_OUTER_BOUND ( 'NONE', #16954, .T. ) ;
#11816 = EDGE_CURVE ( 'NONE', #5578, #1068, #98, .T. ) ;
#11817 = EDGE_CURVE ( 'NONE', #14037, #17029, #15959, .T. ) ;
#11818 = CARTESIAN_POINT ( 'NONE',  ( 3.872354045398264777, 166.6517708494370709, 299.5967279023346350 ) ) ;
#11819 = AXIS2_PLACEMENT_3D ( 'NONE', #6308, #9759, #16775 ) ;
#11820 = VECTOR ( 'NONE', #7907, 1000.000000000000000 ) ;
#11821 = CARTESIAN_POINT ( 'NONE',  ( -55.33808647217894361, 114.8068154851947753, 167.6347561330238420 ) ) ;
#11822 = VERTEX_POINT ( 'NONE', #12311 ) ;
#11823 = CARTESIAN_POINT ( 'NONE',  ( 106.8724933792760226, 79.04398536104964990, 26.04362031086705542 ) ) ;
#11824 = LINE ( 'NONE', #18814, #21059 ) ;
#11825 = VECTOR ( 'NONE', #15774, 1000.000000000000114 ) ;
#11826 = ORIENTED_EDGE ( 'NONE', *, *, #13184, .F. ) ;
#11827 = FACE_OUTER_BOUND ( 'NONE', #10828, .T. ) ;
#11828 = VERTEX_POINT ( 'NONE', #12414 ) ;
#11829 = DIRECTION ( 'NONE',  ( -0.000000000000000000, -1.000000000000000000, -0.000000000000000000 ) ) ;
#11830 = CARTESIAN_POINT ( 'NONE',  ( 7.015576680412777932, 166.1312609306101535, 81.53744875812694204 ) ) ;
#11831 = CARTESIAN_POINT ( 'NONE',  ( 9.002457598320861010, 166.3583706580475621, 81.51051569747208703 ) ) ;
#11832 = CARTESIAN_POINT ( 'NONE',  ( -22.49358496127553053, 324.7653478115767030, 320.5678661935268678 ) ) ;
#11833 = CIRCLE ( 'NONE', #20972, 1.999999999999997558 ) ;
#11834 = DIRECTION ( 'NONE',  ( 0.01292394549866740863, 0.005513023399721176006, 0.9999012842304692006 ) ) ;
#11835 = VECTOR ( 'NONE', #1712, 1000.000000000000114 ) ;
#11836 = TOROIDAL_SURFACE ( 'NONE', #7789, 20.50000000000000355, 2.000000000000000000 ) ;
#11837 = CARTESIAN_POINT ( 'NONE',  ( 1.717753310876226625, 55.00000000000000000, 109.6869605904137330 ) ) ;
#11838 = SHAPE_DEFINITION_REPRESENTATION ( #15656, #16508 ) ;
#11839 = ORIENTED_EDGE ( 'NONE', *, *, #20567, .T. ) ;
#11840 = EDGE_CURVE ( 'NONE', #2734, #15528, #15876, .T. ) ;
#11841 = DIRECTION ( 'NONE',  ( 7.125109674381882011E-05, -0.9999848031710253382, 0.005512562950849702291 ) ) ;
#11842 = VERTEX_POINT ( 'NONE', #5375 ) ;
#11843 = CARTESIAN_POINT ( 'NONE',  ( -84.78539177974977292, 105.0000000000000000, -70.08164767436865361 ) ) ;
#11844 = TOROIDAL_SURFACE ( 'NONE', #11099, 8.000000000000014211, 2.000000000000000000 ) ;
#11845 = DIRECTION ( 'NONE',  ( -5.440186201345785633E-18, -1.000000000000000000, -1.334940939666367878E-17 ) ) ;
#11846 = FACE_OUTER_BOUND ( 'NONE', #505, .T. ) ;
#11847 = CARTESIAN_POINT ( 'NONE',  ( 1.121675378414679125, 105.0000000000000000, 109.9942809619911799 ) ) ;
#11848 = ORIENTED_EDGE ( 'NONE', *, *, #3979, .T. ) ;
#11849 = CARTESIAN_POINT ( 'NONE',  ( 50.67479067645616198, 109.8916839534814471, -44.82796490703182712 ) ) ;
#11850 = ORIENTED_EDGE ( 'NONE', *, *, #17235, .F. ) ;
#11851 = CARTESIAN_POINT ( 'NONE',  ( 85.63433794141033673, 105.0000000000000000, 69.04172771111926465 ) ) ;
#11852 = CARTESIAN_POINT ( 'NONE',  ( -39.99338164115797412, 124.0006990541328804, 0.7705435719247482051 ) ) ;
#11853 = PLANE ( 'NONE',  #6317 ) ;
#11854 = CIRCLE ( 'NONE', #6344, 9.000000000000001776 ) ;
#11855 = ORIENTED_EDGE ( 'NONE', *, *, #2126, .T. ) ;
#11856 = PLANE ( 'NONE',  #859 ) ;
#11857 = CARTESIAN_POINT ( 'NONE',  ( -41.67747345744908216, 165.9786531560170886, 257.1849355913342379 ) ) ;
#11858 = VERTEX_POINT ( 'NONE', #10679 ) ;
#11859 = LINE ( 'NONE', #18524, #3600 ) ;
#11860 = CARTESIAN_POINT ( 'NONE',  ( 49.99582398951007889, 170.0000000000000284, -0.6462070952321007367 ) ) ;
#11861 = EDGE_LOOP ( 'NONE', ( #13098, #18072, #3995 ) ) ;
#11862 = ORIENTED_EDGE ( 'NONE', *, *, #6023, .F. ) ;
#11863 = CARTESIAN_POINT ( 'NONE',  ( -90.13703512730879197, 87.34900181192021762, 51.18604840036999093 ) ) ;
#11864 = AXIS2_PLACEMENT_3D ( 'NONE', #10872, #19360, #21197 ) ;
#11865 = ORIENTED_EDGE ( 'NONE', *, *, #20218, .T. ) ;
#11866 = CARTESIAN_POINT ( 'NONE',  ( -73.50537112628094860, 95.94772729216980167, 81.83508847720149504 ) ) ;
#11867 = CARTESIAN_POINT ( 'NONE',  ( -90.40889375659909888, 72.00000000000000000, 33.17122784026039284 ) ) ;
#11868 = CARTESIAN_POINT ( 'NONE',  ( 1.054933926688728762, 165.4499317482979279, 81.61824794009152129 ) ) ;
#11869 = ORIENTED_EDGE ( 'NONE', *, *, #396, .T. ) ;
#11870 = SURFACE_SIDE_STYLE ('',( #19080 ) ) ;
#11871 = EDGE_CURVE ( 'NONE', #21156, #21267, #9338, .T. ) ;
#11872 = CARTESIAN_POINT ( 'NONE',  ( -88.17224338757175417, 88.87565977966644937, 52.08196082309276420 ) ) ;
#11873 = CARTESIAN_POINT ( 'NONE',  ( 50.81961426468491538, 113.4359159616137731, -44.84937814700944614 ) ) ;
#11874 = CARTESIAN_POINT ( 'NONE',  ( -71.61338682171090397, 92.58578643762702143, -83.49564556265197268 ) ) ;
#11875 = ORIENTED_EDGE ( 'NONE', *, *, #11394, .T. ) ;
#11876 = VERTEX_POINT ( 'NONE', #14498 ) ;
#11877 = DIRECTION ( 'NONE',  ( 0.01292414190464131335, 0.000000000000000000, 0.9999164797902017066 ) ) ;
#11878 = CARTESIAN_POINT ( 'NONE',  ( -3.145996032882572457, 159.0405451880567682, 324.0656923467140018 ) ) ;
#11879 = VECTOR ( 'NONE', #5485, 999.9999999999998863 ) ;
#11880 = CARTESIAN_POINT ( 'NONE',  ( -61.06315242452672010, 118.9229714579762742, 168.3606140555295951 ) ) ;
#11881 = DIRECTION ( 'NONE',  ( 0.01292394549866738261, 0.005513023399722618428, 0.9999012842304692006 ) ) ;
#11882 = CARTESIAN_POINT ( 'NONE',  ( -13.57499642963801634, 147.0376393494719025, 276.9077761425589870 ) ) ;
#11883 = CARTESIAN_POINT ( 'NONE',  ( -55.34016076973275489, 143.9188730675114414, 167.4742716441172377 ) ) ;
#11884 = AXIS2_PLACEMENT_3D ( 'NONE', #12548, #5293, #19312 ) ;
#11885 = VECTOR ( 'NONE', #13381, 1000.000000000000000 ) ;
#11886 = ADVANCED_FACE ( 'NONE', ( #18259 ), #19517, .T. ) ;
#11887 = EDGE_CURVE ( 'NONE', #19122, #3529, #2683, .T. ) ;
#11888 = LINE ( 'NONE', #18874, #9600 ) ;
#11889 = ADVANCED_FACE ( 'NONE', ( #19839 ), #14832, .F. ) ;
#11890 = ORIENTED_EDGE ( 'NONE', *, *, #3594, .F. ) ;
#11891 = VERTEX_POINT ( 'NONE', #10908 ) ;
#11892 = ORIENTED_EDGE ( 'NONE', *, *, #16352, .T. ) ;
#11893 = CARTESIAN_POINT ( 'NONE',  ( -90.04195528733428944, 70.03010874511689110, 63.23285121931508712 ) ) ;
#11894 = ADVANCED_FACE ( 'NONE', ( #18044 ), #7459, .T. ) ;
#11895 = VECTOR ( 'NONE', #11539, 999.9999999999998863 ) ;
#11896 = ORIENTED_EDGE ( 'NONE', *, *, #5020, .T. ) ;
#11897 = CARTESIAN_POINT ( 'NONE',  ( 13.42006642051110177, 160.8124487847600221, 323.5078865155649055 ) ) ;
#11898 = VECTOR ( 'NONE', #12493, 1000.000000000000227 ) ;
#11899 = EDGE_CURVE ( 'NONE', #12967, #10097, #16101, .T. ) ;
#11900 = VECTOR ( 'NONE', #3432, 1000.000000000000000 ) ;
#11901 = CARTESIAN_POINT ( 'NONE',  ( 82.07389037140740129, 75.18483361449105473, 4.863163123076542860 ) ) ;
#11902 = CARTESIAN_POINT ( 'NONE',  ( 79.99331838321626265, 100.9999999999999858, -1.033931352371318058 ) ) ;
#11903 = CARTESIAN_POINT ( 'NONE',  ( -92.21925947168412563, 70.54513337289785113, -59.96440893983639597 ) ) ;
#11904 = EDGE_CURVE ( 'NONE', #18552, #12549, #18151, .T. ) ;
#11905 = DIRECTION ( 'NONE',  ( 0.000000000000000000, 0.000000000000000000, 1.000000000000000000 ) ) ;
#11906 = CARTESIAN_POINT ( 'NONE',  ( 79.99331838321626265, 102.0000000000000000, -6.033931352371315171 ) ) ;
#11907 = LINE ( 'NONE', #3153, #20933 ) ;
#11908 = DIRECTION ( 'NONE',  ( -0.01292394549866738608, -0.005513023399720699824, -0.9999012842304692006 ) ) ;
#11909 = CARTESIAN_POINT ( 'NONE',  ( -51.14300816381444292, 189.5947554187170851, -72.90590013953031701 ) ) ;
#11910 = EDGE_CURVE ( 'NONE', #1991, #1532, #6754, .T. ) ;
#11911 = CARTESIAN_POINT ( 'NONE',  ( 88.42079784105918350, 80.23159800265106867, -32.23730667790416504 ) ) ;
#11912 = ORIENTED_EDGE ( 'NONE', *, *, #11581, .F. ) ;
#11913 = CARTESIAN_POINT ( 'NONE',  ( -69.43142427201328815, 92.58578643762699301, 85.31868097644080251 ) ) ;
#11914 = VECTOR ( 'NONE', #14946, 1000.000000000000000 ) ;
#11915 = EDGE_LOOP ( 'NONE', ( #14327, #7439, #17974, #13355 ) ) ;
#11916 = EDGE_CURVE ( 'NONE', #13637, #9339, #687, .T. ) ;
#11917 = VERTEX_POINT ( 'NONE', #803 ) ;
#11918 = CYLINDRICAL_SURFACE ( 'NONE', #13618, 1.999999999999998446 ) ;
#11919 = CYLINDRICAL_SURFACE ( 'NONE', #16570, 3.399999999999991918 ) ;
#11920 = EDGE_LOOP ( 'NONE', ( #2904, #13088, #135, #4451 ) ) ;
#11921 = VECTOR ( 'NONE', #12124, 999.9999999999998863 ) ;
#11922 = CARTESIAN_POINT ( 'NONE',  ( -109.1029698478473051, 104.3814432989690602, 70.11238825523858509 ) ) ;
#11923 = VERTEX_POINT ( 'NONE', #21783 ) ;
#11924 = VECTOR ( 'NONE', #6592, 1000.000000000000000 ) ;
#11925 = ADVANCED_FACE ( 'NONE', ( #3990 ), #17829, .F. ) ;
#11926 =( REPRESENTATION_RELATIONSHIP ('NONE','NONE', #11808, #15037 ) REPRESENTATION_RELATIONSHIP_WITH_TRANSFORMATION ( #17695 )SHAPE_REPRESENTATION_RELATIONSHIP( ) );
#11927 = LINE ( 'NONE', #4655, #11454 ) ;
#11928 = VECTOR ( 'NONE', #17966, 1000.000000000000000 ) ;
#11929 = VERTEX_POINT ( 'NONE', #7676 ) ;
#11930 = CARTESIAN_POINT ( 'NONE',  ( -0.8096692839990790036, 327.2331353181372720, 317.6013947485918720 ) ) ;
#11931 = PLANE ( 'NONE',  #15897 ) ;
#11932 = EDGE_CURVE ( 'NONE', #1664, #3576, #2361, .T. ) ;
#11933 = ORIENTED_EDGE ( 'NONE', *, *, #4857, .T. ) ;
#11934 = CARTESIAN_POINT ( 'NONE',  ( -10.90995169204228610, 105.6768406389637107, 123.0998174695503451 ) ) ;
#11935 = DIRECTION ( 'NONE',  ( 0.009760756503427813965, -0.9999378516499565217, 0.005387065077607405654 ) ) ;
#11936 = PLANE ( 'NONE',  #11167 ) ;
#11937 = ORIENTED_EDGE ( 'NONE', *, *, #19528, .F. ) ;
#11938 = DIRECTION ( 'NONE',  ( 0.01035335185279129787, 0.005513005182357351951, 0.9999312050732647172 ) ) ;
#11939 = CARTESIAN_POINT ( 'NONE',  ( 51.64670511766545502, 84.99999999999997158, -27.66980033337678790 ) ) ;
#11940 = CARTESIAN_POINT ( 'NONE',  ( -12.63436650347019885, 181.7513824828561440, 322.1994800631134694 ) ) ;
#11941 = CIRCLE ( 'NONE', #14149, 124.0000000000000000 ) ;
#11942 = DIRECTION ( 'NONE',  ( 0.9999164797902015955, -8.863511990578707937E-16, -0.01292414190464158050 ) ) ;
#11943 = EDGE_CURVE ( 'NONE', #6907, #18256, #2292, .T. ) ;
#11944 = CARTESIAN_POINT ( 'NONE',  ( -164.0000000000000000, 18.00000000000000355, -7.999999999999979572 ) ) ;
#11945 = FACE_OUTER_BOUND ( 'NONE', #14635, .T. ) ;
#11946 = DIRECTION ( 'NONE',  ( 0.01292394549866731843, 0.005513023399720594006, 0.9999012842304693116 ) ) ;
#11948 = ORIENTED_EDGE ( 'NONE', *, *, #10086, .T. ) ;
#11947 = ORIENTED_EDGE ( 'NONE', *, *, #22117, .F. ) ;
#11949 = CARTESIAN_POINT ( 'NONE',  ( -55.30663963734144772, 126.9329139721032931, 170.0677384248578790 ) ) ;
#11950 = EDGE_CURVE ( 'NONE', #18464, #3864, #9166, .T. ) ;
#11951 = DIRECTION ( 'NONE',  ( 0.000000000000000000, 0.000000000000000000, 1.000000000000000000 ) ) ;
#11952 = DIRECTION ( 'NONE',  ( -0.9999164797902015955, -6.965998958219364448E-18, 0.01292414190464157182 ) ) ;
#11953 = DIRECTION ( 'NONE',  ( 0.8637520339192008567, 0.002839416958727990648, 0.5039090806998601790 ) ) ;
#11954 = ORIENTED_EDGE ( 'NONE', *, *, #14453, .F. ) ;
#11955 = AXIS2_PLACEMENT_3D ( 'NONE', #3908, #7355, #4247 ) ;
#11956 = CARTESIAN_POINT ( 'NONE',  ( 9.142505149400571796, 81.19615242270661781, -88.65345271381767134 ) ) ;
#11957 = PRODUCT_DEFINITION_SHAPE ( 'NONE', 'NONE',  #22680 ) ;
#11958 = CARTESIAN_POINT ( 'NONE',  ( 9.109368757775373027, 142.0951589094185579, 256.6601876722492648 ) ) ;
#11959 = ORIENTED_EDGE ( 'NONE', *, *, #7131, .T. ) ;
#11960 = CARTESIAN_POINT ( 'NONE',  ( 51.76191778456981751, 109.4814342785208368, -44.83975432626324675 ) ) ;
#11961 = ORIENTED_EDGE ( 'NONE', *, *, #11663, .F. ) ;
#11962 = DIRECTION ( 'NONE',  ( -0.9999164797902015955, -2.001050586450177050E-22, 0.01292414190464223796 ) ) ;
#11963 = CARTESIAN_POINT ( 'NONE',  ( 59.65144567478507298, 126.9191314136042479, 166.0817088952479139 ) ) ;
#11964 = CARTESIAN_POINT ( 'NONE',  ( -27.02995630134907046, 99.74539563421257071, 75.23139667190513080 ) ) ;
#11965 = ORIENTED_EDGE ( 'NONE', *, *, #15355, .F. ) ;
#11966 = DIRECTION ( 'NONE',  ( 0.01292394549866738782, 0.005513023399720700692, 0.9999012842304693116 ) ) ;
#11967 = DIRECTION ( 'NONE',  ( -0.7944560844389294552, 0.000000000000000000, -0.6073216033519345247 ) ) ;
#11968 = ORIENTED_EDGE ( 'NONE', *, *, #14587, .T. ) ;
#11969 = CARTESIAN_POINT ( 'NONE',  ( 48.80621279012751046, 95.32702374722853733, -45.27713056539194270 ) ) ;
#11970 = EDGE_CURVE ( 'NONE', #18877, #9038, #12657, .T. ) ;
#11971 = FACE_OUTER_BOUND ( 'NONE', #9769, .T. ) ;
#11972 = EDGE_CURVE ( 'NONE', #5229, #21242, #2556, .T. ) ;
#11973 = EDGE_LOOP ( 'NONE', ( #1582, #15050, #4416, #19844, #21715, #15721, #16988, #13812 ) ) ;
#11974 = CIRCLE ( 'NONE', #2055, 1.989999999999997105 ) ;
#11975 = CARTESIAN_POINT ( 'NONE',  ( -9.381793152695534488, 81.90747236817703936, -94.06097113112909369 ) ) ;
#11976 = CARTESIAN_POINT ( 'NONE',  ( -88.16578817886077957, 88.47953432603556223, 52.70984377781922348 ) ) ;
#11977 = ORIENTED_EDGE ( 'NONE', *, *, #13839, .T. ) ;
#11978 = ORIENTED_EDGE ( 'NONE', *, *, #19106, .F. ) ;
#11979 = CARTESIAN_POINT ( 'NONE',  ( -10.88352610546617250, 183.4880351429991379, 323.0108604666241376 ) ) ;
#11980 = DIRECTION ( 'NONE',  ( 7.125109674159586684E-05, -0.9999848031710252272, 0.005512562950848869624 ) ) ;
#11981 = DIRECTION ( 'NONE',  ( 0.4910069343201003411, -0.004767316193522950878, -0.8711426192914036859 ) ) ;
#11982 = DIRECTION ( 'NONE',  ( 0.01035335185279115042, 0.005513005182354825326, 0.9999312050732648283 ) ) ;
#11983 = CARTESIAN_POINT ( 'NONE',  ( -61.79544715037562241, 127.3639955235004777, 248.3502612411157315 ) ) ;
#11984 = CARTESIAN_POINT ( 'NONE',  ( -70.91392079944854743, 91.17157287525390075, -84.09052168258642723 ) ) ;
#11985 = ORIENTED_EDGE ( 'NONE', *, *, #22525, .T. ) ;
#11986 = ORIENTED_EDGE ( 'NONE', *, *, #22220, .F. ) ;
#11987 = DIRECTION ( 'NONE',  ( 0.01292394549866728373, 0.005513023399720296501, 0.9999012842304693116 ) ) ;
#11988 = DIRECTION ( 'NONE',  ( -0.6080604969667605664, -0.004419696743559108250, -0.7938783901261144971 ) ) ;
#11989 = DIRECTION ( 'NONE',  ( 0.9999164797902015955, 6.965998958219364448E-18, -0.01292414190464157182 ) ) ;
#11990 = CYLINDRICAL_SURFACE ( 'NONE', #14761, 4.199999999999997513 ) ;
#11991 = DIRECTION ( 'NONE',  ( 7.125109674364536131E-05, -0.9999848031710253382, 0.005512562950849705760 ) ) ;
#11992 = DIRECTION ( 'NONE',  ( 1.000000000000000000, 0.000000000000000000, 0.000000000000000000 ) ) ;
#11993 = CYLINDRICAL_SURFACE ( 'NONE', #925, 2.499999999999988010 ) ;
#11994 = CARTESIAN_POINT ( 'NONE',  ( 89.90836385050337753, 100.2819950034553926, 63.37719018575645435 ) ) ;
#11995 = ADVANCED_FACE ( 'NONE', ( #1368 ), #10074, .F. ) ;
#11996 = CARTESIAN_POINT ( 'NONE',  ( -164.0000000000000000, 1.999999999999998224, 53.76161406891260697 ) ) ;
#11997 = ORIENTED_EDGE ( 'NONE', *, *, #16815, .T. ) ;
#11998 = ORIENTED_EDGE ( 'NONE', *, *, #15005, .T. ) ;
#11999 = ORIENTED_EDGE ( 'NONE', *, *, #21407, .T. ) ;
#12000 = CARTESIAN_POINT ( 'NONE',  ( 92.43457499998882554, 77.12912189496645965, -31.19724316448930423 ) ) ;
#12001 = CYLINDRICAL_SURFACE ( 'NONE', #5436, 120.0000000000000000 ) ;
#12002 = CARTESIAN_POINT ( 'NONE',  ( -55.40268456415264353, 18.00000000000000355, -113.1659955246495883 ) ) ;
#12003 = DIRECTION ( 'NONE',  ( -0.01292394549866744159, -0.005513023399721009472, -0.9999012842304692006 ) ) ;
#12004 = EDGE_CURVE ( 'NONE', #5453, #8420, #11357, .T. ) ;
#12005 = DIRECTION ( 'NONE',  ( 0.8981428216242005602, -3.051058334780146661E-15, -0.4397038457472480788 ) ) ;
#12006 = ORIENTED_EDGE ( 'NONE', *, *, #16172, .F. ) ;
#12007 = PRESENTATION_STYLE_ASSIGNMENT (( #22533 ) ) ;
#12008 = DIRECTION ( 'NONE',  ( 0.000000000000000000, 0.000000000000000000, 1.000000000000000000 ) ) ;
#12009 = LINE ( 'NONE', #4749, #131 ) ;
#12010 = DIRECTION ( 'NONE',  ( 0.9999164797902017066, 6.965998958219365988E-18, -0.01292414190464157356 ) ) ;
#12011 = CARTESIAN_POINT ( 'NONE',  ( 9.997142846107600178, 175.3350937402613852, 324.1393829572561458 ) ) ;
#12012 = DIRECTION ( 'NONE',  ( 0.01292394549866743812, 0.005513023399720639109, 0.9999012842304693116 ) ) ;
#12013 = ORIENTED_EDGE ( 'NONE', *, *, #4318, .T. ) ;
#12014 = CIRCLE ( 'NONE', #17519, 112.5000000000000142 ) ;
#12015 = DIRECTION ( 'NONE',  ( -0.01292394549866745720, -0.005513023399720816918, -0.9999012842304692006 ) ) ;
#12016 = CARTESIAN_POINT ( 'NONE',  ( -8.508136329860027658, 185.4226668845482209, 305.1523461349310082 ) ) ;
#12017 = EDGE_LOOP ( 'NONE', ( #9899, #14496, #2936, #11234 ) ) ;
#12018 = CARTESIAN_POINT ( 'NONE',  ( -89.22767861003021039, 80.31838830481380853, -30.18953644180660945 ) ) ;
#12019 = EDGE_CURVE ( 'NONE', #11631, #1653, #6073, .T. ) ;
#12020 = ORIENTED_EDGE ( 'NONE', *, *, #7097, .T. ) ;
#12021 = EDGE_CURVE ( 'NONE', #9861, #9560, #6422, .T. ) ;
#12022 = CARTESIAN_POINT ( 'NONE',  ( -9.064738643541179641, 105.7168211570308500, 130.3284763332909222 ) ) ;
#12023 = ORIENTED_EDGE ( 'NONE', *, *, #8286, .T. ) ;
#12024 = CARTESIAN_POINT ( 'NONE',  ( -90.40889375659909888, 69.99999999999998579, 33.17122784026039284 ) ) ;
#12025 = DIRECTION ( 'NONE',  ( 0.7161863329816251511, 0.003898296230782347105, 0.6978982302147139771 ) ) ;
#12026 = EDGE_CURVE ( 'NONE', #1318, #2070, #12698, .T. ) ;
#12027 = CYLINDRICAL_SURFACE ( 'NONE', #11109, 3.099999999999998757 ) ;
#12028 = VERTEX_POINT ( 'NONE', #2748 ) ;
#12029 = CIRCLE ( 'NONE', #21186, 2.000000000000004441 ) ;
#12030 = EDGE_CURVE ( 'NONE', #11876, #7316, #10095, .T. ) ;
#12031 = CARTESIAN_POINT ( 'NONE',  ( 13.67035244215019851, 187.1120429933681351, 322.8635577162621644 ) ) ;
#12032 = ADVANCED_FACE ( 'NONE', ( #9645 ), #4663, .F. ) ;
#12033 = PLANE ( 'NONE',  #20148 ) ;
#12034 = CARTESIAN_POINT ( 'NONE',  ( 108.6051929143323065, 76.36431273661730756, -17.61389195241292782 ) ) ;
#12035 = CARTESIAN_POINT ( 'NONE',  ( -164.0000000000000000, 18.00000000000000355, 53.76161406891260697 ) ) ;
#12036 = ORIENTED_EDGE ( 'NONE', *, *, #5813, .T. ) ;
#12037 = AXIS2_PLACEMENT_3D ( 'NONE', #11520, #2996, #22046 ) ;
#12038 = LINE ( 'NONE', #3290, #12545 ) ;
#12039 = B_SPLINE_CURVE_WITH_KNOTS ( 'NONE', 3,
 ( #17616, #12559, #14286, #19431, #8733, #10715, #19208, #3692, #10837, #8632, #28, #13934, #16133, #17860, #3479, #10492 ),
 .UNSPECIFIED., .F., .F.,
 ( 4, 2, 2, 2, 2, 2, 2, 4 ),
 ( 0.000000000000000000, 0.0004728798714926100619, 0.0009457597429852201238, 0.001418639614477830132, 0.001891519485970440248, 0.002364399357463050581, 0.002837279228955660263, 0.003783038971940870521 ),
 .UNSPECIFIED. ) ;
#12040 = DIRECTION ( 'NONE',  ( 7.125109674161259066E-05, -0.9999848031710252272, 0.005512562950850163727 ) ) ;
#12041 = LINE ( 'NONE', #3293, #3674 ) ;
#12042 = STYLED_ITEM ( 'NONE', ( #2817 ), #1960 ) ;
#12043 = APPLICATION_CONTEXT ( 'automotive_design' ) ;
#12044 = CARTESIAN_POINT ( 'NONE',  ( 19.55320478417725738, 183.1354159283349929, 318.8669710253166159 ) ) ;
#12045 = EDGE_CURVE ( 'NONE', #16756, #3247, #16774, .T. ) ;
#12046 = DIRECTION ( 'NONE',  ( -0.9999164797902015955, -4.476705744456278510E-15, 0.01292414190463697134 ) ) ;
#12047 = CARTESIAN_POINT ( 'NONE',  ( -10.73300451425737734, 335.5619885905173305, 328.3571198817161303 ) ) ;
#12048 = EDGE_CURVE ( 'NONE', #14615, #11284, #7909, .T. ) ;
#12049 = CARTESIAN_POINT ( 'NONE',  ( -164.0000000000000000, 18.00000000000000355, 4.016841501203319170E-14 ) ) ;
#12050 = CARTESIAN_POINT ( 'NONE',  ( -14.52969038923042966, 137.6261247937603969, 113.8584785293034400 ) ) ;
#12051 = ITEM_DEFINED_TRANSFORMATION ( 'NONE', 'NONE', #13613,  #6292 ) ;
#12052 = AXIS2_PLACEMENT_3D ( 'NONE', #12944, #6140, #983 ) ;
#12054 = VERTEX_POINT ( 'NONE', #4778 ) ;
#12053 = VERTEX_POINT ( 'NONE', #21890 ) ;
#12055 = CARTESIAN_POINT ( 'NONE',  ( 3.898201936395599532, 166.6627968962365287, 301.5965304707955852 ) ) ;
#12056 = PLANE ( 'NONE',  #4306 ) ;
#12057 = CARTESIAN_POINT ( 'NONE',  ( -68.71681667565952978, 69.99999999999998579, 85.89527988174785378 ) ) ;
#12058 = AXIS2_PLACEMENT_3D ( 'NONE', #7482, #5740, #9420 ) ;
#12059 = AXIS2_PLACEMENT_3D ( 'NONE', #1307, #4823, #961 ) ;
#12060 = CARTESIAN_POINT ( 'NONE',  ( -56.11438623100832501, 126.5883500096206262, 107.5739081604536693 ) ) ;
#12061 = ORIENTED_EDGE ( 'NONE', *, *, #2259, .F. ) ;
#12062 = ORIENTED_EDGE ( 'NONE', *, *, #20170, .F. ) ;
#12063 = DIRECTION ( 'NONE',  ( 7.125109674364534776E-05, -0.9999848031710252272, 0.005512562950849704893 ) ) ;
#12064 = CARTESIAN_POINT ( 'NONE',  ( -51.54031057290245599, 113.3115871737369673, -43.52566795857408266 ) ) ;
#12065 = VERTEX_POINT ( 'NONE', #6186 ) ;
#12066 = EDGE_CURVE ( 'NONE', #7339, #2719, #11824, .T. ) ;
#12067 = CARTESIAN_POINT ( 'NONE',  ( 51.66853286597432771, 109.8098455164457619, -44.84035802310724250 ) ) ;
#12068 = ORIENTED_EDGE ( 'NONE', *, *, #11216, .T. ) ;
#12069 = DIRECTION ( 'NONE',  ( 0.000000000000000000, 0.000000000000000000, 1.000000000000000000 ) ) ;
#12070 =( BOUNDED_SURFACE ( )  B_SPLINE_SURFACE ( 3, 2, ( 
 ( #22068, #13828, #6372 ),
 ( #19090, #15339, #1430 ),
 ( #20812, #6582, #10041 ),
 ( #4627, #18977, #13393 ),
 ( #15114, #17273, #16829 ),
 ( #1324, #6482, #5067 ),
 ( #13723, #3235, #11650 ),
 ( #12104, #10153, #13496 ),
 ( #10259, #6698, #8306 ),
 ( #1539, #1211, #18644 ),
 ( #17158, #22292, #8523 ),
 ( #11882, #2909, #20470 ),
 ( #4726, #11762, #22514 ),
 ( #15564, #20706, #18871 ) ),
 .UNSPECIFIED., .F., .F., .T. ) 
 B_SPLINE_SURFACE_WITH_KNOTS ( ( 4, 2, 2, 2, 2, 2, 4 ),
 ( 3, 3 ),
 ( -0.01502904264599872093, -0.01127178198449904113, -0.007514521322999362200, -0.005635890992249522301, -0.003757260661499682835, -0.001878630330749843152, -3.469446951953614189E-18 ),
 ( 0.000000000000000000, 1.000000000000000000 ),
 .UNSPECIFIED. ) 
 GEOMETRIC_REPRESENTATION_ITEM ( )  RATIONAL_B_SPLINE_SURFACE ( (
 ( 1.000000000000000000, 1.000000000000000000, 1.000000000000000000),
 ( 1.000000000000000000, 0.9999832193749498277, 1.000000000000000000),
 ( 1.000000000000000000, 0.9943958665421850363, 1.000000000000000000),
 ( 1.000000000000000000, 0.9719875995013427250, 1.000000000000000000),
 ( 1.000000000000000000, 0.9551974090680757090, 1.000000000000000000),
 ( 1.000000000000000000, 0.9207014414829839399, 1.000000000000000000),
 ( 1.000000000000000000, 0.9076211955268852494, 1.000000000000000000),
 ( 1.000000000000000000, 0.8785736512504284113, 1.000000000000000000),
 ( 1.000000000000000000, 0.8625652577300224610, 1.000000000000000000),
 ( 1.000000000000000000, 0.8274118182163137103, 1.000000000000000000),
 ( 1.000000000000000000, 0.8082693262191131822, 1.000000000000000000),
 ( 1.000000000000000000, 0.7665332262313664380, 1.000000000000000000),
 ( 1.000000000000000000, 0.7439399906329980938, 1.000000000000000000),
 ( 1.000000000000000000, 0.7193398003386509698, 1.000000000000000000) ) ) 
 REPRESENTATION_ITEM ( '' )  SURFACE ( )  );
#12071 = CARTESIAN_POINT ( 'NONE',  ( 106.2089377515398780, 77.28919246392754872, 28.62973177816271431 ) ) ;
#12072 = DIRECTION ( 'NONE',  ( 2.025474946048326158E-22, -1.000000000000000000, 1.876735158486679638E-22 ) ) ;
#12073 = FACE_BOUND ( 'NONE', #17915, .T. ) ;
#12074 = CARTESIAN_POINT ( 'NONE',  ( -2.536883864190021320, 327.0424951675884131, 319.3070269798304253 ) ) ;
#12075 = CARTESIAN_POINT ( 'NONE',  ( -8.879611143719925437, 165.4774968652964731, 86.74699578029056113 ) ) ;
#12076 = VERTEX_POINT ( 'NONE', #18484 ) ;
#12077 = EDGE_CURVE ( 'NONE', #2761, #8205, #15732, .T. ) ;
#12078 = AXIS2_PLACEMENT_3D ( 'NONE', #9766, #6193, #11369 ) ;
#12079 = ORIENTED_EDGE ( 'NONE', *, *, #16606, .F. ) ;
#12080 = CARTESIAN_POINT ( 'NONE',  ( 90.37009694938035409, 70.86971351442876710, -62.71573865539092907 ) ) ;
#12081 = CARTESIAN_POINT ( 'NONE',  ( -90.05797812368525967, 88.60843922159206443, 52.63312143047516400 ) ) ;
#12082 = DIRECTION ( 'NONE',  ( 0.9934404589540163366, 0.1135548637187052401, -0.01346653032743036320 ) ) ;
#12083 = EDGE_LOOP ( 'NONE', ( #700, #3965, #2584, #6449 ) ) ;
#12084 = VERTEX_POINT ( 'NONE', #16879 ) ;
#12085 = PLANE ( 'NONE',  #2981 ) ;
#12086 = CLOSED_SHELL ( 'NONE', ( #20066, #10096, #8630, #5768, #19460, #20853, #8746, #19493, #14881, #8275, #16687, #5798, #21140, #14197, #10351, #21332, #13149, #4437, #19294, #2881, #22513, #4216, #5135, #10406, #10796, #3856, #20312, #10558, #2672, #6415, #14292, #21357, #10217, #3549, #267, #20637, #11766, #8093 ) ) ;
#12087 = LINE ( 'NONE', #8393, #5570 ) ;
#12088 = CARTESIAN_POINT ( 'NONE',  ( -4.843581286828654520, 86.22336876296598973, -75.02848097551373030 ) ) ;
#12089 = ORIENTED_EDGE ( 'NONE', *, *, #13782, .F. ) ;
#12090 = CARTESIAN_POINT ( 'NONE',  ( -12.72332588857627300, 326.2897452428853740, 421.4431498403059777 ) ) ;
#12091 = VECTOR ( 'NONE', #20515, 1000.000000000000114 ) ;
#12092 = DIRECTION ( 'NONE',  ( 0.9999164797902015955, 2.001050586450177050E-22, -0.01292414190464223796 ) ) ;
#12093 = DIRECTION ( 'NONE',  ( -7.125109674161230605E-05, 0.9999848031710253382, -0.005512562950850140309 ) ) ;
#12094 = VERTEX_POINT ( 'NONE', #15171 ) ;
#12095 = EDGE_CURVE ( 'NONE', #8665, #18197, #19591, .T. ) ;
#12096 = ORIENTED_EDGE ( 'NONE', *, *, #3895, .F. ) ;
#12097 = EDGE_CURVE ( 'NONE', #10294, #12028, #21430, .T. ) ;
#12098 = AXIS2_PLACEMENT_3D ( 'NONE', #8924, #15971, #3532 ) ;
#12099 = ORIENTED_EDGE ( 'NONE', *, *, #6740, .T. ) ;
#12100 = FACE_OUTER_BOUND ( 'NONE', #4513, .T. ) ;
#12101 = FACE_OUTER_BOUND ( 'NONE', #7285, .T. ) ;
#12102 = DIRECTION ( 'NONE',  ( -0.01292394549866704608, -0.005513023399720698957, -0.9999012842304692006 ) ) ;
#12103 = CARTESIAN_POINT ( 'NONE',  ( 40.57355171551004247, 108.0982075334647163, 198.8652726751216733 ) ) ;
#12104 = CARTESIAN_POINT ( 'NONE',  ( -10.48163666083949863, 145.5635402874828230, 276.5713533137832769 ) ) ;
#12105 = DIRECTION ( 'NONE',  ( 0.000000000000000000, 0.000000000000000000, 1.000000000000000000 ) ) ;
#12106 = SURFACE_STYLE_FILL_AREA ( #7155 ) ;
#12107 = CARTESIAN_POINT ( 'NONE',  ( -51.21962256273560854, 114.2039301678666874, 164.7922289650441883 ) ) ;
#12108 = CARTESIAN_POINT ( 'NONE',  ( -157.5176307659779127, 0.000000000000000000, 60.94675664190624786 ) ) ;
#12109 = EDGE_LOOP ( 'NONE', ( #21462, #20082, #9807, #5731 ) ) ;
#12110 = AXIS2_PLACEMENT_3D ( 'NONE', #12750, #14600, #18040 ) ;
#12111 = EDGE_LOOP ( 'NONE', ( #21039, #8918, #13150, #10971, #2571, #8052, #19191, #5216, #7144, #22269 ) ) ;
#12112 = CONICAL_SURFACE ( 'NONE', #20875, 3.399999999999986144, 1.029744258676653201 ) ;
#12113 = CYLINDRICAL_SURFACE ( 'NONE', #6037, 1.999999999999997780 ) ;
#12114 = AXIS2_PLACEMENT_3D ( 'NONE', #9030, #11344, #325 ) ;
#12115 = ORIENTED_EDGE ( 'NONE', *, *, #11768, .T. ) ;
#12116 = CONICAL_SURFACE ( 'NONE', #18000, 5.010000000000001563, 0.9599310885968744822 ) ;
#12117 = LINE ( 'NONE', #13949, #15377 ) ;
#12118 = DIRECTION ( 'NONE',  ( 0.01297756288283796570, 0.000000000000000000, 0.9999157878849708192 ) ) ;
#12119 = CARTESIAN_POINT ( 'NONE',  ( -146.5000000000000000, 20.00000000000000000, 2.081668171172168513E-14 ) ) ;
#12120 = EDGE_CURVE ( 'NONE', #18358, #367, #4911, .T. ) ;
#12121 = DIRECTION ( 'NONE',  ( 0.000000000000000000, 1.000000000000000000, 0.000000000000000000 ) ) ;
#12122 = FACE_OUTER_BOUND ( 'NONE', #6818, .T. ) ;
#12123 = CARTESIAN_POINT ( 'NONE',  ( 11.95378257394767196, 187.7068342974569362, 304.8847554649954645 ) ) ;
#12124 = DIRECTION ( 'NONE',  ( 7.125109674160258889E-05, -0.9999848031710253382, 0.005512562950849898315 ) ) ;
#12125 = CIRCLE ( 'NONE', #2207, 2.000000000000000000 ) ;
#12126 = PRESENTATION_LAYER_ASSIGNMENT (  '', '', ( #5127 ) ) ;
#12127 = CARTESIAN_POINT ( 'NONE',  ( -56.47028073308179330, 114.1922624142001581, 162.7435536389593267 ) ) ;
#12128 = AXIS2_PLACEMENT_3D ( 'NONE', #14614, #19972, #2423 ) ;
#12129 = FACE_OUTER_BOUND ( 'NONE', #144, .T. ) ;
#12130 = AXIS2_PLACEMENT_3D ( 'NONE', #6250, #16496, #16833 ) ;
#12131 = CARTESIAN_POINT ( 'NONE',  ( 41.42451162475439475, 125.7553391191873544, -44.79586833841344173 ) ) ;
#12132 = VERTEX_POINT ( 'NONE', #10538 ) ;
#12133 = CARTESIAN_POINT ( 'NONE',  ( 8.627475644446743530, 70.55908004698135016, -87.97989623083630306 ) ) ;
#12134 = ORIENTED_EDGE ( 'NONE', *, *, #7185, .F. ) ;
#12135 = AXIS2_PLACEMENT_3D ( 'NONE', #3134, #18758, #9922 ) ;
#12136 = PRODUCT_DEFINITION_SHAPE ( 'NONE', 'NONE',  #22670 ) ;
#12137 = CIRCLE ( 'NONE', #6269, 6.499999999999998224 ) ;
#12138 = FACE_OUTER_BOUND ( 'NONE', #12383, .T. ) ;
#12139 = AXIS2_PLACEMENT_3D ( 'NONE', #1494, #15521, #22471 ) ;
#12140 = EDGE_LOOP ( 'NONE', ( #15748, #13677, #458, #9290 ) ) ;
#12141 = FACE_BOUND ( 'NONE', #20244, .T. ) ;
#12142 = PRESENTATION_STYLE_ASSIGNMENT (( #17436 ) ) ;
#12143 = FACE_OUTER_BOUND ( 'NONE', #2118, .T. ) ;
#12144 = VECTOR ( 'NONE', #14903, 1000.000000000000114 ) ;
#12145 = EDGE_LOOP ( 'NONE', ( #14505, #20668, #16907, #9413, #20910, #4713, #16498, #21472 ) ) ;
#12146 = CARTESIAN_POINT ( 'NONE',  ( -12.86548928906161571, 326.2291019854885121, 410.4442357137708086 ) ) ;
#12147 = ORIENTED_EDGE ( 'NONE', *, *, #3881, .F. ) ;
#12148 = CARTESIAN_POINT ( 'NONE',  ( 64.02527527396304663, 169.5865232450209703, -75.83266554108695345 ) ) ;
#12149 = EDGE_CURVE ( 'NONE', #1745, #17283, #8575, .T. ) ;
#12150 = CARTESIAN_POINT ( 'NONE',  ( 106.8378915622753880, 78.29428632475668337, -26.20941106207498095 ) ) ;
#12151 = CARTESIAN_POINT ( 'NONE',  ( 54.52327687265660927, 0.000000000000000000, 111.3697098814019029 ) ) ;
#12152 = ADVANCED_FACE ( 'NONE', ( #20980 ), #11936, .T. ) ;
#12153 = CARTESIAN_POINT ( 'NONE',  ( -7.094262839591980452, 165.3861282783320803, 296.7451558832441378 ) ) ;
#12154 = EDGE_LOOP ( 'NONE', ( #20263, #16206, #22415, #2882 ) ) ;
#12155 = DIRECTION ( 'NONE',  ( -0.01292394549866727679, -0.005513023399720742325, -0.9999012842304692006 ) ) ;
#12156 = AXIS2_PLACEMENT_3D ( 'NONE', #8682, #15731, #5240 ) ;
#12157 = VERTEX_POINT ( 'NONE', #12035 ) ;
#12158 = PRODUCT_DEFINITION_SHAPE ( 'NONE', 'NONE',  #1029 ) ;
#12159 = DIRECTION ( 'NONE',  ( -0.9934404589540163366, -0.1135548637187057258, 0.01346653032743036146 ) ) ;
#12160 = DIRECTION ( 'NONE',  ( 0.9999464000778708339, 1.417269118681874529E-05, -0.01035358732233823860 ) ) ;
#12161 = DIRECTION ( 'NONE',  ( -0.01292394549866731669, -0.005513023399720593139, -0.9999012842304692006 ) ) ;
#12162 = AXIS2_PLACEMENT_3D ( 'NONE', #4025, #18187, #7711 ) ;
#12163 = CARTESIAN_POINT ( 'NONE',  ( 12.85102440982953809, 187.3455989732921694, 304.9938768930631454 ) ) ;
#12164 = EDGE_CURVE ( 'NONE', #14649, #17187, #9715, .T. ) ;
#12165 = AXIS2_PLACEMENT_3D ( 'NONE', #7888, #16755, #16526 ) ;
#12166 = CARTESIAN_POINT ( 'NONE',  ( -2.322807172541347498, 69.99999999999998579, -81.06750429846923112 ) ) ;
#12167 = CARTESIAN_POINT ( 'NONE',  ( -39.36913080622078809, 69.99999999999998579, 87.51612159803859470 ) ) ;
#12168 = CARTESIAN_POINT ( 'NONE',  ( 54.52327687265662348, 0.000000000000000000, -111.3697098814019313 ) ) ;
#12169 = DIRECTION ( 'NONE',  ( 0.01292394549866738608, 0.005513023399720699824, 0.9999012842304692006 ) ) ;
#12170 = EDGE_CURVE ( 'NONE', #18473, #20719, #1639, .T. ) ;
#12171 = CONTEXT_DEPENDENT_SHAPE_REPRESENTATION ( #1043, #5338 ) ;
#12172 = LINE ( 'NONE', #15740, #15816 ) ;
#12173 = VECTOR ( 'NONE', #2878, 1000.000000000000114 ) ;
#12174 = ORIENTED_EDGE ( 'NONE', *, *, #13562, .F. ) ;
#12175 = CARTESIAN_POINT ( 'NONE',  ( -35.70966223998150468, 93.64690829566262664, 83.82160924485184239 ) ) ;
#12176 = CARTESIAN_POINT ( 'NONE',  ( -48.56675489936627343, 108.6799603325455763, -43.53856503602677464 ) ) ;
#12177 = DIRECTION ( 'NONE',  ( -0.3102455404053308108, -0.9506564598521405340, 0.000000000000000000 ) ) ;
#12178 = LINE ( 'NONE', #16090, #10301 ) ;
#12179 = CARTESIAN_POINT ( 'NONE',  ( 13.80509744631564750, 155.5569384583423300, 100.8921482990249956 ) ) ;
#12180 = VECTOR ( 'NONE', #8964, 1000.000000000000000 ) ;
#12181 = EDGE_CURVE ( 'NONE', #564, #1989, #22337, .T. ) ;
#12182 = ORIENTED_EDGE ( 'NONE', *, *, #17200, .F. ) ;
#12183 = CARTESIAN_POINT ( 'NONE',  ( -83.58290648752343088, 104.4142135623730780, -71.51152175067954886 ) ) ;
#12184 = CARTESIAN_POINT ( 'NONE',  ( -6.702556532201366046, 81.99999999999998579, -87.68700545388549017 ) ) ;
#12185 = ORIENTED_EDGE ( 'NONE', *, *, #1383, .T. ) ;
#12186 = EDGE_CURVE ( 'NONE', #9319, #5759, #10198, .T. ) ;
#12187 = CARTESIAN_POINT ( 'NONE',  ( 48.60502302639385874, 111.9953525209499645, -44.81281142087428293 ) ) ;
#12188 = CONICAL_SURFACE ( 'NONE', #17707, 5.999999999999951150, 0.7853981633974415066 ) ;
#12189 = VERTEX_POINT ( 'NONE', #20644 ) ;
#12190 = CARTESIAN_POINT ( 'NONE',  ( 106.2880716433167976, 78.18499655656310665, 28.33463432393087089 ) ) ;
#12191 = DIRECTION ( 'NONE',  ( -0.01292394549866745720, -0.005513023399720816918, -0.9999012842304692006 ) ) ;
#12192 = LINE ( 'NONE', #19290, #4085 ) ;
#12193 = ADVANCED_FACE ( 'NONE', ( #18918 ), #10440, .T. ) ;
#12194 = ORIENTED_EDGE ( 'NONE', *, *, #6115, .T. ) ;
#12195 = CARTESIAN_POINT ( 'NONE',  ( 49.99582398951007889, 170.0000000000000284, -0.6462070952321007367 ) ) ;
#12196 = LINE ( 'NONE', #4934, #18177 ) ;
#12197 = AXIS2_PLACEMENT_3D ( 'NONE', #9294, #8017, #15049 ) ;
#12198 = VERTEX_POINT ( 'NONE', #12153 ) ;
#12199 = CIRCLE ( 'NONE', #449, 7.499999999999992006 ) ;
#12200 = CARTESIAN_POINT ( 'NONE',  ( 21.95462417325102322, 168.7812190940428536, 314.8544026679174408 ) ) ;
#12201 = CARTESIAN_POINT ( 'NONE',  ( 14.28523666940072978, 188.7757037738094255, 275.4832468541452499 ) ) ;
#12202 = ORIENTED_EDGE ( 'NONE', *, *, #4318, .F. ) ;
#12203 = CARTESIAN_POINT ( 'NONE',  ( 64.07473967894682687, 103.0000000000000000, -72.00569783435743432 ) ) ;
#12204 = CARTESIAN_POINT ( 'NONE',  ( -89.90032551572470254, 87.88518503742774612, 50.85709393580534510 ) ) ;
#12205 = EDGE_CURVE ( 'NONE', #3828, #20395, #4182, .T. ) ;
#12206 = VECTOR ( 'NONE', #2538, 1000.000000000000114 ) ;
#12207 = PLANE ( 'NONE',  #22127 ) ;
#12208 = ORIENTED_EDGE ( 'NONE', *, *, #6918, .F. ) ;
#12209 = ORIENTED_EDGE ( 'NONE', *, *, #15684, .F. ) ;
#12210 = CARTESIAN_POINT ( 'NONE',  ( -74.36685259725942387, 95.85792126150981574, 81.05301575120802227 ) ) ;
#12211 =( BOUNDED_CURVE ( )  B_SPLINE_CURVE ( 3, ( #9299, #7578, #19847, #7466 ),
 .UNSPECIFIED., .F., .T. ) 
 B_SPLINE_CURVE_WITH_KNOTS ( ( 4, 4 ),
 ( 0.000000000000000000, 1.570796326794896558 ),
 .UNSPECIFIED. ) 
 CURVE ( )  GEOMETRIC_REPRESENTATION_ITEM ( )  RATIONAL_B_SPLINE_CURVE ( ( 1.000000000000000000, 0.8047378541243649375, 0.8047378541243649375, 1.000000000000000000 ) ) 
 REPRESENTATION_ITEM ( '' )  );
#12212 = DIRECTION ( 'NONE',  ( 0.01292394549866734098, 0.005513023399720419666, 0.9999012842304692006 ) ) ;
#12213 = ORIENTED_EDGE ( 'NONE', *, *, #6869, .T. ) ;
#12214 = CIRCLE ( 'NONE', #2298, 9.921742784567037177 ) ;
#12215 = CARTESIAN_POINT ( 'NONE',  ( 84.94669401314519064, 75.00864948959271317, 0.2251543083152826030 ) ) ;
#12216 = CIRCLE ( 'NONE', #8173, 1.999999999999997335 ) ;
#12217 = CARTESIAN_POINT ( 'NONE',  ( 64.31563894222803413, 189.7102623349352086, -53.44515082906027459 ) ) ;
#12218 = ORIENTED_EDGE ( 'NONE', *, *, #21684, .T. ) ;
#12219 = ADVANCED_FACE ( 'NONE', ( #17448, #21095 ), #8454, .F. ) ;
#12220 = VERTEX_POINT ( 'NONE', #3417 ) ;
#12221 = DIRECTION ( 'NONE',  ( -7.125109674160325297E-05, 0.9999848031710253382, -0.005512562950849327591 ) ) ;
#12222 = CARTESIAN_POINT ( 'NONE',  ( -79.39043653009960622, 75.13519862315604314, -4.041203518313574605 ) ) ;
#12223 = CARTESIAN_POINT ( 'NONE',  ( -28.46703706805638134, 324.0603700370125466, 315.1514505861725866 ) ) ;
#12224 = FACE_OUTER_BOUND ( 'NONE', #22560, .T. ) ;
#12225 = ORIENTED_EDGE ( 'NONE', *, *, #2, .F. ) ;
#12226 = AXIS2_PLACEMENT_3D ( 'NONE', #7326, #14370, #570 ) ;
#12227 = CARTESIAN_POINT ( 'NONE',  ( -65.90110554552374822, 105.0000000000000000, -69.29678410920486442 ) ) ;
#12228 = CARTESIAN_POINT ( 'NONE',  ( 0.2404759814345563407, 168.6025580852140422, 18.60517306324423004 ) ) ;
#12229 = ORIENTED_EDGE ( 'NONE', *, *, #4444, .T. ) ;
#12230 = VECTOR ( 'NONE', #19829, 1000.000000000000114 ) ;
#12231 = EDGE_LOOP ( 'NONE', ( #14640, #3777, #18792 ) ) ;
#12232 = AXIS2_PLACEMENT_3D ( 'NONE', #4656, #8335, #22111 ) ;
#12233 = B_SPLINE_CURVE_WITH_KNOTS ( 'NONE', 3,
 ( #21697, #2660, #5859, #13020 ),
 .UNSPECIFIED., .F., .F.,
 ( 4, 4 ),
 ( 0.1567379737884350144, 0.1627913398252618660 ),
 .UNSPECIFIED. ) ;
#12234 = CARTESIAN_POINT ( 'NONE',  ( 19.15702598245626831, 184.5830064527947059, 311.5659919418918093 ) ) ;
#12235 = EDGE_CURVE ( 'NONE', #14141, #6788, #10312, .T. ) ;
#12236 = ORIENTED_EDGE ( 'NONE', *, *, #18209, .F. ) ;
#12237 = DIRECTION ( 'NONE',  ( 7.125109674161246868E-05, -0.9999848031710253382, 0.005512562950850155054 ) ) ;
#12238 = CARTESIAN_POINT ( 'NONE',  ( 91.86813470756436573, 77.17527876199572745, -31.26628371047692667 ) ) ;
#12239 = CIRCLE ( 'NONE', #16313, 3.399999999999986144 ) ;
#12240 = DIRECTION ( 'NONE',  ( -0.01292414190464131335, -1.902755938799530239E-22, -0.9999164797902015955 ) ) ;
#12241 = CARTESIAN_POINT ( 'NONE',  ( -38.93830720113543009, 95.97017003981163441, 82.39966276358782693 ) ) ;
#12242 = DIRECTION ( 'NONE',  ( 0.1296504907605108559, 0.005475273188901296634, 0.9915446392518419971 ) ) ;
#12243 = CARTESIAN_POINT ( 'NONE',  ( -64.99457118636308905, 169.9999999999999716, 0.8400692238016759239 ) ) ;
#12244 = CARTESIAN_POINT ( 'NONE',  ( 11.85672047603351054, 187.7744756917181803, 307.7628753140074309 ) ) ;
#12245 = AXIS2_PLACEMENT_3D ( 'NONE', #3623, #21309, #1918 ) ;
#12246 = CARTESIAN_POINT ( 'NONE',  ( 10.07658213627836119, 175.6783734781009798, 323.8030538038543682 ) ) ;
#12247 = VECTOR ( 'NONE', #21522, 999.9999999999998863 ) ;
#12248 = CARTESIAN_POINT ( 'NONE',  ( 14.23917046504717021, 105.7413430127404439, 134.4755589474307840 ) ) ;
#12249 = VERTEX_POINT ( 'NONE', #12276 ) ;
#12250 = CARTESIAN_POINT ( 'NONE',  ( -36.90283430563165723, 95.89798883583559075, 85.13120909300619132 ) ) ;
#12251 = FACE_OUTER_BOUND ( 'NONE', #21159, .T. ) ;
#12252 = VERTEX_POINT ( 'NONE', #8676 ) ;
#12253 = CIRCLE ( 'NONE', #19218, 110.0000000000000142 ) ;
#12254 = CARTESIAN_POINT ( 'NONE',  ( -93.21002351426727728, 77.12912189496638860, -28.79774562292281814 ) ) ;
#12255 = ORIENTED_EDGE ( 'NONE', *, *, #17979, .T. ) ;
#12256 = ADVANCED_FACE ( 'NONE', ( #6744 ), #13027, .T. ) ;
#12257 = EDGE_CURVE ( 'NONE', #17518, #5334, #3087, .T. ) ;
#12258 = AXIS2_PLACEMENT_3D ( 'NONE', #16822, #13712, #3225 ) ;
#12259 = AXIS2_PLACEMENT_3D ( 'NONE', #21623, #15126, #4066 ) ;
#12260 = CARTESIAN_POINT ( 'NONE',  ( -64.99457118636308905, 105.0000000000000000, 0.8400692238016757019 ) ) ;
#12261 =( NAMED_UNIT ( * ) PLANE_ANGLE_UNIT ( ) SI_UNIT ( $, .RADIAN. ) );
#12262 = PRODUCT_DEFINITION_CONTEXT ( 'detailed design', #6173, 'design' ) ;
#12263 = ORIENTED_EDGE ( 'NONE', *, *, #17039, .T. ) ;
#12264 = CARTESIAN_POINT ( 'NONE',  ( -54.68979215835705077, 114.2467007792763098, 172.5957179600166569 ) ) ;
#12265 =( NAMED_UNIT ( * ) PLANE_ANGLE_UNIT ( ) SI_UNIT ( $, .RADIAN. ) );
#12266 = CARTESIAN_POINT ( 'NONE',  ( -2.503839020269049254, 159.3664414540641587, 324.7217779040802270 ) ) ;
#12267 = VERTEX_POINT ( 'NONE', #1807 ) ;
#12268 = CARTESIAN_POINT ( 'NONE',  ( 13.02613253520115499, 190.3084650069641839, 320.8516703567468085 ) ) ;
#12269 = ORIENTED_EDGE ( 'NONE', *, *, #1658, .T. ) ;
#12270 = ORIENTED_EDGE ( 'NONE', *, *, #7366, .F. ) ;
#12271 = VECTOR ( 'NONE', #19960, 999.9999999999998863 ) ;
#12272 = DIRECTION ( 'NONE',  ( 7.125109674364534776E-05, -0.9999848031710252272, 0.005512562950849704893 ) ) ;
#12273 = PRODUCT_DEFINITION ( 'UNKNOWN', '', #770, #5572 ) ;
#12274 = DIRECTION ( 'NONE',  ( 0.01292414190464131508, 3.469447142229204684E-15, 0.9999164797902017066 ) ) ;
#12275 = CARTESIAN_POINT ( 'NONE',  ( -9.663116041263174694, 184.4449190506678633, 323.1798533313222492 ) ) ;
#12277 = DIRECTION ( 'NONE',  ( -0.9999164797902015955, 0.000000000000000000, 0.01292414190464162733 ) ) ;
#12276 = CARTESIAN_POINT ( 'NONE',  ( -56.85872436582616274, 143.2710928180442522, 49.98587074703709732 ) ) ;
#12278 = CIRCLE ( 'NONE', #3077, 4.199999999999997513 ) ;
#12279 = ORIENTED_EDGE ( 'NONE', *, *, #7267, .F. ) ;
#12280 = DIRECTION ( 'NONE',  ( 0.9934404589540163366, 0.1135548637187061005, -0.01346653032743037014 ) ) ;
#12281 = CIRCLE ( 'NONE', #8241, 4.000000000000006217 ) ;
#12282 = CARTESIAN_POINT ( 'NONE',  ( -90.64608739977010998, 77.80075968338644543, 32.24365086765050847 ) ) ;
#12283 = CARTESIAN_POINT ( 'NONE',  ( -64.99457118636308905, 177.0000000000003695, 0.8400692238016794766 ) ) ;
#12284 = DIRECTION ( 'NONE',  ( 0.009760756503427813965, -0.9999378516499565217, 0.005387065077607405654 ) ) ;
#12285 = ORIENTED_EDGE ( 'NONE', *, *, #8979, .F. ) ;
#12286 = ORIENTED_EDGE ( 'NONE', *, *, #17071, .T. ) ;
#12287 = ADVANCED_FACE ( 'NONE', ( #19025 ), #8792, .F. ) ;
#12288 = CARTESIAN_POINT ( 'NONE',  ( 18.46966468191076416, 183.9248624754537502, 308.3369342292732540 ) ) ;
#12289 = DIRECTION ( 'NONE',  ( -0.9999164797902017066, 7.828075210616901716E-16, 0.01292414190464158050 ) ) ;
#12290 = AXIS2_PLACEMENT_3D ( 'NONE', #21458, #2167, #16339 ) ;
#12291 = CARTESIAN_POINT ( 'NONE',  ( -70.91392079944854743, 69.99999999999998579, -84.09052168258642723 ) ) ;
#12292 = VERTEX_POINT ( 'NONE', #12499 ) ;
#12293 = EDGE_CURVE ( 'NONE', #7332, #555, #16311, .T. ) ;
#12294 = DIRECTION ( 'NONE',  ( 0.01292394549866695240, 0.005513023399718316314, 0.9999012842304693116 ) ) ;
#12295 = LINE ( 'NONE', #19273, #5200 ) ;
#12296 = ITEM_DEFINED_TRANSFORMATION ( 'NONE', 'NONE', #11772,  #6292 ) ;
#12297 = AXIS2_PLACEMENT_3D ( 'NONE', #10106, #2973, #4674 ) ;
#12298 = CARTESIAN_POINT ( 'NONE',  ( -10.92353791676496222, 113.6640392289254322, 120.7557495267353147 ) ) ;
#12299 = DIRECTION ( 'NONE',  ( -2.025474946048326158E-22, 1.000000000000000000, -1.876735158486679638E-22 ) ) ;
#12300 = DIRECTION ( 'NONE',  ( 0.9999164797902017066, 6.965998958219365988E-18, -0.01292414190464157356 ) ) ;
#12301 = CARTESIAN_POINT ( 'NONE',  ( -157.5176307659779411, 0.000000000000000000, -60.94675664190620523 ) ) ;
#12302 = ORIENTED_EDGE ( 'NONE', *, *, #15632, .T. ) ;
#12303 = ORIENTED_EDGE ( 'NONE', *, *, #2852, .F. ) ;
#12304 = LINE ( 'NONE', #22583, #16029 ) ;
#12305 = DIRECTION ( 'NONE',  ( 7.125109674364534776E-05, -0.9999848031710252272, 0.005512562950849704893 ) ) ;
#12306 = ADVANCED_FACE ( 'NONE', ( #14469 ), #6499, .T. ) ;
#12307 = ORIENTED_EDGE ( 'NONE', *, *, #2609, .F. ) ;
#12308 = CARTESIAN_POINT ( 'NONE',  ( 48.12047892932057636, 111.2511799747316559, -44.80244553543491293 ) ) ;
#12309 = VERTEX_POINT ( 'NONE', #5460 ) ;
#12310 = CARTESIAN_POINT ( 'NONE',  ( 158.3970384574715808, 18.00000000000000355, -62.74304228515678261 ) ) ;
#12311 = CARTESIAN_POINT ( 'NONE',  ( 14.80019909389238464, 167.9008743503427468, 299.4485960687320585 ) ) ;
#12312 = CIRCLE ( 'NONE', #563, 2.000000000000001332 ) ;
#12313 = DIRECTION ( 'NONE',  ( 0.9909299940865190504, -0.1338359446631136318, -0.01207007604876911971 ) ) ;
#12314 = CARTESIAN_POINT ( 'NONE',  ( 37.54386652542171277, 92.77591188308413450, 82.72434418715882032 ) ) ;
#12315 = EDGE_CURVE ( 'NONE', #20578, #13213, #16075, .T. ) ;
#12316 = DIRECTION ( 'NONE',  ( -0.01292394549866739996, -0.005513023399721131770, -0.9999012842304692006 ) ) ;
#12317 = LINE ( 'NONE', #1731, #1676 ) ;
#12318 = EDGE_LOOP ( 'NONE', ( #19912, #17404, #17900, #22389, #9254, #2578 ) ) ;
#12319 = CARTESIAN_POINT ( 'NONE',  ( -0.5070102419236742763, 327.2655426976345439, 317.0551077940115192 ) ) ;
#12320 = FACE_OUTER_BOUND ( 'NONE', #21078, .T. ) ;
#12321 = ORIENTED_EDGE ( 'NONE', *, *, #3315, .T. ) ;
#12322 = EDGE_CURVE ( 'NONE', #8095, #3357, #16648, .T. ) ;
#12323 = CARTESIAN_POINT ( 'NONE',  ( -51.42433909778522150, 169.3906321239456361, -109.8753121617313724 ) ) ;
#12324 = CARTESIAN_POINT ( 'NONE',  ( -89.99979403183252202, 87.72028009250037428, 50.95876237836445455 ) ) ;
#12325 = ADVANCED_FACE ( 'NONE', ( #18569 ), #7887, .T. ) ;
#12326 = ORIENTED_EDGE ( 'NONE', *, *, #9253, .F. ) ;
#12327 = ORIENTED_EDGE ( 'NONE', *, *, #2641, .T. ) ;
#12328 = CARTESIAN_POINT ( 'NONE',  ( -34.79726985247908999, 121.2962013336460814, 248.0347590154626971 ) ) ;
#12329 = CARTESIAN_POINT ( 'NONE',  ( -51.19775092088617185, 169.4872888238259634, -92.34461233820157133 ) ) ;
#12330 =( LENGTH_UNIT ( ) NAMED_UNIT ( * ) SI_UNIT ( .MILLI., .METRE. ) );
#12331 = DIRECTION ( 'NONE',  ( -0.1136178953597579422, 0.9935164314186355483, -0.004009283626633659663 ) ) ;
#12332 = CARTESIAN_POINT ( 'NONE',  ( -64.99457118636311748, 170.0000000000008242, 0.8400692238025471159 ) ) ;
#12333 = EDGE_CURVE ( 'NONE', #9403, #20163, #4856, .T. ) ;
#12334 = ORIENTED_EDGE ( 'NONE', *, *, #19870, .T. ) ;
#12335 = LINE ( 'NONE', #13626, #16517 ) ;
#12336 = ORIENTED_EDGE ( 'NONE', *, *, #6196, .T. ) ;
#12337 = LINE ( 'NONE', #17613, #1623 ) ;
#12338 = CARTESIAN_POINT ( 'NONE',  ( -75.38806545726168906, 75.02669947309938436, 3.231589135580875904 ) ) ;
#12339 = CARTESIAN_POINT ( 'NONE',  ( -13.74451874060598122, 164.7026647133428980, 315.8397882698648687 ) ) ;
#12340 = DIRECTION ( 'NONE',  ( 0.01292394549866731149, 0.005513023399720593139, 0.9999012842304692006 ) ) ;
#12341 = ADVANCED_FACE ( 'NONE', ( #22098 ), #3394, .T. ) ;
#12342 = CARTESIAN_POINT ( 'NONE',  ( 68.19355272015712899, 129.3639651298425406, 246.6590976676106095 ) ) ;
#12343 = DIRECTION ( 'NONE',  ( 7.125109674364536131E-05, -0.9999848031710253382, 0.005512562950849705760 ) ) ;
#12344 = CIRCLE ( 'NONE', #17865, 4.000000000000002665 ) ;
#12345 = CYLINDRICAL_SURFACE ( 'NONE', #5509, 2.000000000000004885 ) ;
#12346 = ORIENTED_EDGE ( 'NONE', *, *, #13604, .T. ) ;
#12347 = PRODUCT_DEFINITION_SHAPE ( 'NONE', 'NONE',  #22679 ) ;
#12348 = CARTESIAN_POINT ( 'NONE',  ( 163.9999999999998863, 20.00000000000000000, 8.000000000002229328 ) ) ;
#12349 = VERTEX_POINT ( 'NONE', #7772 ) ;
#12350 = ORIENTED_EDGE ( 'NONE', *, *, #17659, .T. ) ;
#12351 = ORIENTED_EDGE ( 'NONE', *, *, #19091, .T. ) ;
#12352 = CARTESIAN_POINT ( 'NONE',  ( 16.68734734459444269, 187.6588240762195028, 319.6336511773113784 ) ) ;
#12353 = ADVANCED_FACE ( 'NONE', ( #21865 ), #4424, .F. ) ;
#12354 = ORIENTED_EDGE ( 'NONE', *, *, #16149, .F. ) ;
#12355 = CARTESIAN_POINT ( 'NONE',  ( -146.5000000000000000, 20.00000000000000000, -9.999999999999980460 ) ) ;
#12356 = DIRECTION ( 'NONE',  ( 0.01292394549866738261, 0.005513023399721051106, 0.9999012842304692006 ) ) ;
#12357 = DIRECTION ( 'NONE',  ( 0.009760756503428008254, -0.9999378516499564107, 0.005387065077611006073 ) ) ;
#12358 = FACE_OUTER_BOUND ( 'NONE', #6070, .T. ) ;
#12359 = CARTESIAN_POINT ( 'NONE',  ( -40.72903392649028120, 95.05466328596200754, 83.34854290912163322 ) ) ;
#12360 = PRODUCT_DEFINITION_SHAPE ( 'NONE', 'NONE',  #9870 ) ;
#12361 = ORIENTED_EDGE ( 'NONE', *, *, #16268, .F. ) ;
#12362 = CARTESIAN_POINT ( 'NONE',  ( -89.85940970469351896, 88.83791317007154476, 86.46162627816347879 ) ) ;
#12363 = CARTESIAN_POINT ( 'NONE',  ( 82.31479625729774341, 75.17608775817923572, -6.847477558719483604 ) ) ;
#12364 = CARTESIAN_POINT ( 'NONE',  ( 15.35300465305828510, 186.1419466745651334, 308.1514022875052774 ) ) ;
#12365 = CARTESIAN_POINT ( 'NONE',  ( 92.80269534486838268, 79.83421200779717708, 28.82571798309749056 ) ) ;
#12366 =( REPRESENTATION_RELATIONSHIP ('NONE','NONE', #11808, #19567 ) REPRESENTATION_RELATIONSHIP_WITH_TRANSFORMATION ( #566 )SHAPE_REPRESENTATION_RELATIONSHIP( ) );
#12367 = CYLINDRICAL_SURFACE ( 'NONE', #1496, 2.000000000000004441 ) ;
#12368 = EDGE_CURVE ( 'NONE', #4404, #21811, #13321, .T. ) ;
#12369 = ORIENTED_EDGE ( 'NONE', *, *, #1101, .F. ) ;
#12370 = CARTESIAN_POINT ( 'NONE',  ( -8.447676300393007764, 185.5761720159400738, 322.6786239791117623 ) ) ;
#12371 = DIRECTION ( 'NONE',  ( -7.125109674141484573E-05, 0.9999848031710252272, -0.005512562950865663482 ) ) ;
#12372 = ORIENTED_EDGE ( 'NONE', *, *, #58, .F. ) ;
#12373 = CARTESIAN_POINT ( 'NONE',  ( -91.37189824458694432, 79.16991425845397146, -26.65847270750067111 ) ) ;
#12374 = VERTEX_POINT ( 'NONE', #9739 ) ;
#12375 = EDGE_CURVE ( 'NONE', #18579, #4119, #11334, .T. ) ;
#12376 = AXIS2_PLACEMENT_3D ( 'NONE', #18508, #16792, #18605 ) ;
#12377 = DIRECTION ( 'NONE',  ( -0.01292394549866632963, -0.005513023399716958026, -0.9999012842304692006 ) ) ;
#12378 = CARTESIAN_POINT ( 'NONE',  ( -44.75608623905984729, 173.1024896994836979, 19.16195291567427716 ) ) ;
#12379 = CARTESIAN_POINT ( 'NONE',  ( -38.68617183816869698, 163.9153776386440882, 273.1592279730091377 ) ) ;
#12380 = PLANE ( 'NONE',  #20287 ) ;
#12381 = VERTEX_POINT ( 'NONE', #18336 ) ;
#12382 = CARTESIAN_POINT ( 'NONE',  ( 12.37582071282576024, 188.2881946015995709, 320.9507921273384454 ) ) ;
#12383 = EDGE_LOOP ( 'NONE', ( #15031, #21661, #21437, #18362 ) ) ;
#12384 = CARTESIAN_POINT ( 'NONE',  ( -22.49358496127894824, 324.7653478115763050, 320.5678661935266973 ) ) ;
#12385 = VECTOR ( 'NONE', #3985, 1000.000000000000114 ) ;
#12386 = CARTESIAN_POINT ( 'NONE',  ( 3.872354045398203937, 166.6517708494369856, 299.5967279023338392 ) ) ;
#12387 = EDGE_CURVE ( 'NONE', #9306, #10904, #8534, .T. ) ;
#12388 = ORIENTED_EDGE ( 'NONE', *, *, #676, .F. ) ;
#12389 = DIRECTION ( 'NONE',  ( -0.5848048290265493998, 0.5741585497524471782, -0.5730141985094219237 ) ) ;
#12390 = EDGE_CURVE ( 'NONE', #6708, #8567, #1242, .T. ) ;
#12391 = DIRECTION ( 'NONE',  ( -0.01292394549866750231, -0.005513023399722823126, -0.9999012842304692006 ) ) ;
#12392 = DIRECTION ( 'NONE',  ( 0.000000000000000000, -1.000000000000000000, 0.000000000000000000 ) ) ;
#12393 = EDGE_LOOP ( 'NONE', ( #18441, #8585, #14601, #5877 ) ) ;
#12394 = CARTESIAN_POINT ( 'NONE',  ( -51.44976785811018516, 169.3797848675314128, -111.8426873806957502 ) ) ;
#12395 = CARTESIAN_POINT ( 'NONE',  ( -49.99582398951010731, 170.0000000000000284, 0.6462070952320568828 ) ) ;
#12396 = CARTESIAN_POINT ( 'NONE',  ( -20.57130763759250414, 139.7551263635816952, -44.07174742163757486 ) ) ;
#12397 = CARTESIAN_POINT ( 'NONE',  ( -14.77271874809119900, 178.9768699339249451, 318.9195234373038375 ) ) ;
#12398 = DIRECTION ( 'NONE',  ( 0.9999164797902015955, 8.772500386246549315E-18, -0.01292414190464155101 ) ) ;
#12399 = CARTESIAN_POINT ( 'NONE',  ( -0.1457028305847437588, 70.14698466122824527, -80.78463022974995056 ) ) ;
#12400 = CONICAL_SURFACE ( 'NONE', #12772, 5.999999999999951150, 0.7853981633974415066 ) ;
#12401 = CARTESIAN_POINT ( 'NONE',  ( -1.163172771417702478, 86.00000000000001421, -89.99248318111824574 ) ) ;
#12402 = ORIENTED_EDGE ( 'NONE', *, *, #3358, .F. ) ;
#12403 = CARTESIAN_POINT ( 'NONE',  ( 1.458023040593673859E-15, 0.000000000000000000, 9.999999999999994671 ) ) ;
#12404 = CARTESIAN_POINT ( 'NONE',  ( -10.89787692332478386, 335.2519218263954599, 322.6332997474033277 ) ) ;
#12405 = CARTESIAN_POINT ( 'NONE',  ( 49.99582398951007889, 170.0000000000000284, -0.6462070952321007367 ) ) ;
#12406 = CARTESIAN_POINT ( 'NONE',  ( 3.316611465012865967, 166.4147053302257007, 256.5999727791399323 ) ) ;
#12407 = CIRCLE ( 'NONE', #1032, 102.6746853779045381 ) ;
#12408 = ORIENTED_EDGE ( 'NONE', *, *, #9193, .T. ) ;
#12409 = DIRECTION ( 'NONE',  ( -0.000000000000000000, 1.000000000000000000, -0.000000000000000000 ) ) ;
#12410 = CARTESIAN_POINT ( 'NONE',  ( 90.02055463237803679, 72.00000000000000000, -63.21629334023821656 ) ) ;
#12411 = ORIENTED_EDGE ( 'NONE', *, *, #12030, .F. ) ;
#12412 = FACE_OUTER_BOUND ( 'NONE', #11020, .T. ) ;
#12413 = ORIENTED_EDGE ( 'NONE', *, *, #19667, .F. ) ;
#12414 = CARTESIAN_POINT ( 'NONE',  ( -5.929909278051283650, 86.00000000000001421, -93.63641280122985222 ) ) ;
#12415 = FACE_OUTER_BOUND ( 'NONE', #8488, .T. ) ;
#12416 = CARTESIAN_POINT ( 'NONE',  ( -49.99582398951009310, 170.0000000000008242, 0.6462070952329234119 ) ) ;
#12417 = AXIS2_PLACEMENT_3D ( 'NONE', #7677, #21558, #4111 ) ;
#12418 = CARTESIAN_POINT ( 'NONE',  ( 58.10057221494500368, 126.2575686056377435, 46.09355478759161429 ) ) ;
#12419 = FACE_OUTER_BOUND ( 'NONE', #14596, .T. ) ;
#12420 = ORIENTED_EDGE ( 'NONE', *, *, #13529, .F. ) ;
#12421 = AXIS2_PLACEMENT_3D ( 'NONE', #9356, #13164, #14553 ) ;
#12422 = FACE_OUTER_BOUND ( 'NONE', #19703, .T. ) ;
#12423 = EDGE_CURVE ( 'NONE', #19859, #979, #20995, .T. ) ;
#12424 = CARTESIAN_POINT ( 'NONE',  ( -90.06162176126106544, 87.58759337840020009, 51.04022814688357812 ) ) ;
#12425 = EDGE_LOOP ( 'NONE', ( #8123, #21330, #2987 ) ) ;
#12426 = AXIS2_PLACEMENT_3D ( 'NONE', #15686, #390, #2108 ) ;
#12427 = ORIENTED_EDGE ( 'NONE', *, *, #6824, .T. ) ;
#12428 = CARTESIAN_POINT ( 'NONE',  ( 64.99457118636310327, 170.0000000000000284, -0.8400692238017243296 ) ) ;
#12429 = DIRECTION ( 'NONE',  ( 0.9934404589540163366, 0.1135548637187057813, -0.01346653032742924430 ) ) ;
#12430 = DIRECTION ( 'NONE',  ( 0.01292394549866738782, 0.005513023399720468239, 0.9999012842304692006 ) ) ;
#12431 = CARTESIAN_POINT ( 'NONE',  ( 84.36058151735579713, 75.03814149158517921, 1.605125682363267803 ) ) ;
#12432 = EDGE_CURVE ( 'NONE', #21267, #21156, #19895, .T. ) ;
#12433 = FACE_BOUND ( 'NONE', #5539, .T. ) ;
#12434 = ORIENTED_EDGE ( 'NONE', *, *, #14980, .T. ) ;
#12435 = DIRECTION ( 'NONE',  ( 0.000000000000000000, 0.000000000000000000, 1.000000000000000000 ) ) ;
#12436 = ORIENTED_EDGE ( 'NONE', *, *, #5551, .F. ) ;
#12437 = CARTESIAN_POINT ( 'NONE',  ( 48.52820596802476416, 171.1607679754053208, 275.9924097807974022 ) ) ;
#12438 = CARTESIAN_POINT ( 'NONE',  ( -63.91682626075579066, 94.48610424851698042, 84.22316112083726125 ) ) ;
#12439 = CARTESIAN_POINT ( 'NONE',  ( -76.83013909114643525, 75.08639547911839429, 5.048240262065343487 ) ) ;
#12440 = CARTESIAN_POINT ( 'NONE',  ( -11.29548081222967326, 164.9574442151662197, 309.5726054092390314 ) ) ;
#12441 = TOROIDAL_SURFACE ( 'NONE', #1057, 97.00000000000004263, 2.000000000000000000 ) ;
#12442 = ADVANCED_FACE ( 'NONE', ( #15027 ), #9837, .T. ) ;
#12443 = ORIENTED_EDGE ( 'NONE', *, *, #7661, .F. ) ;
#12444 = ADVANCED_FACE ( 'NONE', ( #13306 ), #20387, .T. ) ;
#12445 = DIRECTION ( 'NONE',  ( -1.396592535537253658E-14, 0.000000000000000000, -1.000000000000000000 ) ) ;
#12446 = CARTESIAN_POINT ( 'NONE',  ( -39.56633482716346606, 107.3157093434689244, 71.90145589903634971 ) ) ;
#12447 = SURFACE_SIDE_STYLE ('',( #5408 ) ) ;
#12448 = VECTOR ( 'NONE', #10419, 1000.000000000000000 ) ;
#12449 = DIRECTION ( 'NONE',  ( 0.9999164797902017066, 6.965998958219365988E-18, -0.01292414190464157356 ) ) ;
#12450 = ORIENTED_EDGE ( 'NONE', *, *, #17355, .T. ) ;
#12451 = FACE_BOUND ( 'NONE', #20432, .T. ) ;
#12452 = ORIENTED_EDGE ( 'NONE', *, *, #16832, .T. ) ;
#12453 = ORIENTED_EDGE ( 'NONE', *, *, #11556, .F. ) ;
#12454 = UNCERTAINTY_MEASURE_WITH_UNIT (LENGTH_MEASURE( 1.000000000000000082E-05 ), #3037, 'distance_accuracy_value', 'NONE');
#12455 = EDGE_CURVE ( 'NONE', #10325, #7269, #7742, .T. ) ;
#12456 = DIRECTION ( 'NONE',  ( -1.387778780781445676E-14, 0.000000000000000000, -1.000000000000000000 ) ) ;
#12457 = ADVANCED_FACE ( 'NONE', ( #14288 ), #10493, .T. ) ;
#12458 = AXIS2_PLACEMENT_3D ( 'NONE', #9680, #8177, #20222 ) ;
#12459 = VERTEX_POINT ( 'NONE', #1757 ) ;
#12460 = EDGE_CURVE ( 'NONE', #17368, #11196, #11204, .T. ) ;
#12461 = AXIS2_PLACEMENT_3D ( 'NONE', #1154, #4342, #2645 ) ;
#12462 = DIRECTION ( 'NONE',  ( 0.01292394549866740169, 0.005513023399720822990, 0.9999012842304693116 ) ) ;
#12463 = CARTESIAN_POINT ( 'NONE',  ( 3.545303425248414353, 81.34441321561124028, -91.95213924926606808 ) ) ;
#12464 = DIRECTION ( 'NONE',  ( -0.000000000000000000, -1.000000000000000000, -0.000000000000000000 ) ) ;
#12465 = DIRECTION ( 'NONE',  ( 0.01292394549866738782, 0.005513023399720468239, 0.9999012842304692006 ) ) ;
#12466 = DIRECTION ( 'NONE',  ( 0.01292394549866737741, 0.005513023399721125699, 0.9999012842304693116 ) ) ;
#12467 = CARTESIAN_POINT ( 'NONE',  ( 12.66469053819756496, 187.4244128634429956, 304.9628814567714699 ) ) ;
#12468 = CARTESIAN_POINT ( 'NONE',  ( 91.22751156961064112, 80.31838830481379432, 30.16368815799726733 ) ) ;
#12469 = EDGE_CURVE ( 'NONE', #1373, #12267, #9110, .T. ) ;
#12470 = EDGE_CURVE ( 'NONE', #19122, #11172, #19433, .T. ) ;
#12472 = DIRECTION ( 'NONE',  ( 7.125109674364534776E-05, -0.9999848031710252272, 0.005512562950849704893 ) ) ;
#12471 = B_SPLINE_CURVE_WITH_KNOTS ( 'NONE', 3,
 ( #4274, #4504, #6239, #6122, #4050, #13265, #7616, #14655, #18303, #4384, #11299, #9225, #16612, #12929 ),
 .UNSPECIFIED., .F., .F.,
 ( 4, 2, 2, 2, 2, 2, 4 ),
 ( 0.000000000000000000, 0.0005169893790259184321, 0.001033978758051836864, 0.001550968137077755188, 0.002067957516103673728, 0.003101936274155510376, 0.004135915032207347457 ),
 .UNSPECIFIED. ) ;
#12473 = CIRCLE ( 'NONE', #9524, 11.78759343285143224 ) ;
#12474 = PRESENTATION_LAYER_ASSIGNMENT (  '', '', ( #8763 ) ) ;
#12475 = CARTESIAN_POINT ( 'NONE',  ( 92.43457499998882554, 69.99999999999998579, -31.19724316448930779 ) ) ;
#12476 = CARTESIAN_POINT ( 'NONE',  ( 59.61913581103840443, 126.9053488551049611, 163.5819556846717546 ) ) ;
#12477 = CIRCLE ( 'NONE', #8419, 8.000000000000014211 ) ;
#12478 = ORIENTED_EDGE ( 'NONE', *, *, #10393, .T. ) ;
#12479 = CARTESIAN_POINT ( 'NONE',  ( -89.98285967923901296, 79.53265832318567163, -27.83436926225114050 ) ) ;
#12480 = ORIENTED_EDGE ( 'NONE', *, *, #20997, .F. ) ;
#12481 = EDGE_CURVE ( 'NONE', #5755, #3063, #11854, .T. ) ;
#12482 = LINE ( 'NONE', #15493, #21289 ) ;
#12483 = ADVANCED_FACE ( 'NONE', ( #2097 ), #14415, .T. ) ;
#12484 = DIRECTION ( 'NONE',  ( -0.01292394549866741557, -0.005513023399720270480, -0.9999012842304693116 ) ) ;
#12485 = VECTOR ( 'NONE', #4477, 1000.000000000000114 ) ;
#12486 = DIRECTION ( 'NONE',  ( 0.009088227368120111588, 0.7109943316365107124, 0.7031390079522377157 ) ) ;
#12487 = VECTOR ( 'NONE', #15204, 999.9999999999998863 ) ;
#12488 = APPLICATION_CONTEXT ( 'automotive_design' ) ;
#12489 = CARTESIAN_POINT ( 'NONE',  ( 163.9999999999998863, 1.999999999999998224, 8.000000000002229328 ) ) ;
#12490 = EDGE_LOOP ( 'NONE', ( #1736, #10607, #6418, #19202 ) ) ;
#12491 = DIRECTION ( 'NONE',  ( 0.01292414190464131335, 0.000000000000000000, 0.9999164797902017066 ) ) ;
#12492 = DIRECTION ( 'NONE',  ( -0.7968670734554590407, -0.4220031449644014443, 0.4323380770678043605 ) ) ;
#12493 = DIRECTION ( 'NONE',  ( -0.02100262710018138690, 0.02843993988601859271, -0.9993748343210220320 ) ) ;
#12494 = EDGE_CURVE ( 'NONE', #21319, #12292, #1992, .T. ) ;
#12495 = DIRECTION ( 'NONE',  ( 0.9934404589540162256, 0.1135548637187056842, -0.01346653032743081423 ) ) ;
#12496 = VERTEX_POINT ( 'NONE', #8981 ) ;
#12497 = CARTESIAN_POINT ( 'NONE',  ( -11.49273635071671862, 182.9480784776224880, 322.8740417677803407 ) ) ;
#12498 = AXIS2_PLACEMENT_3D ( 'NONE', #12853, #9638, #911 ) ;
#12499 = CARTESIAN_POINT ( 'NONE',  ( -44.49054948644865703, 166.4747265717734308, 273.2201396957804036 ) ) ;
#12500 = CARTESIAN_POINT ( 'NONE',  ( -1.163172771417702700, 69.99999999999998579, -89.99248318111824574 ) ) ;
#12501 = ORIENTED_EDGE ( 'NONE', *, *, #18824, .F. ) ;
#12502 = CARTESIAN_POINT ( 'NONE',  ( -12.72040503869455286, 184.6056756926249989, 309.1932742806828287 ) ) ;
#12503 = FACE_BOUND ( 'NONE', #10012, .T. ) ;
#12504 = CARTESIAN_POINT ( 'NONE',  ( -3.646887971868283618, 326.8692299522281814, 307.8272933952192716 ) ) ;
#12505 = CARTESIAN_POINT ( 'NONE',  ( -14.49142894009190741, 179.3925286715590346, 319.5713301818169043 ) ) ;
#12506 = AXIS2_PLACEMENT_3D ( 'NONE', #6750, #17334, #12284 ) ;
#12507 = CARTESIAN_POINT ( 'NONE',  ( 19.43357779880557601, 183.2511996782348547, 319.0807864945002166 ) ) ;
#12508 = VECTOR ( 'NONE', #18223, 1000.000000000000114 ) ;
#12509 = ORIENTED_EDGE ( 'NONE', *, *, #511, .T. ) ;
#12510 = DIRECTION ( 'NONE',  ( -5.440186201345738641E-18, -1.000000000000000000, -1.334940939666364181E-17 ) ) ;
#12511 = ADVANCED_FACE ( 'NONE', ( #21160 ), #374, .T. ) ;
#12512 = VECTOR ( 'NONE', #13854, 1000.000000000000114 ) ;
#12513 = ADVANCED_FACE ( 'NONE', ( #7369 ), #19321, .F. ) ;
#12514 = DIRECTION ( 'NONE',  ( 1.000000000000000000, -0.000000000000000000, -1.458023040593674599E-16 ) ) ;
#12515 = CARTESIAN_POINT ( 'NONE',  ( -11.19296010916491824, 157.5998335170374389, 101.2039900878849750 ) ) ;
#12516 = LINE ( 'NONE', #16329, #472 ) ;
#12517 = ORIENTED_EDGE ( 'NONE', *, *, #17659, .F. ) ;
#12518 = ORIENTED_EDGE ( 'NONE', *, *, #4969, .F. ) ;
#12519 = CARTESIAN_POINT ( 'NONE',  ( -57.55221044392004615, 114.6951352185433421, 172.9675203174990088 ) ) ;
#12520 = DIRECTION ( 'NONE',  ( 0.01292394549866731843, 0.005513023399720594006, 0.9999012842304693116 ) ) ;
#12521 = CIRCLE ( 'NONE', #15471, 4.374999999999991118 ) ;
#12522 = EDGE_LOOP ( 'NONE', ( #12218, #18623, #15821, #2685 ) ) ;
#12523 = DIRECTION ( 'NONE',  ( 1.490566292661454305E-14, 1.000000000000000000, -1.926591840573834312E-16 ) ) ;
#12524 = ORIENTED_EDGE ( 'NONE', *, *, #15632, .F. ) ;
#12525 = CARTESIAN_POINT ( 'NONE',  ( 48.26972705805141572, 171.0505075074109129, 255.9943840961880710 ) ) ;
#12526 = AXIS2_PLACEMENT_3D ( 'NONE', #15644, #20671, #1294 ) ;
#12527 = CARTESIAN_POINT ( 'NONE',  ( -49.64894119642055870, 126.1473026246197406, 27.48387445644694083 ) ) ;
#12528 = AXIS2_PLACEMENT_3D ( 'NONE', #13827, #4958, #1209 ) ;
#12529 = DIRECTION ( 'NONE',  ( -0.01292414190464049456, -1.752983723092351571E-15, -0.9999164797902015955 ) ) ;
#12530 = CARTESIAN_POINT ( 'NONE',  ( -64.64767546932803555, 126.1473081376431082, 27.67873648630081362 ) ) ;
#12531 = CARTESIAN_POINT ( 'NONE',  ( 17.15867526775164720, 146.4158769158963196, 277.8065902176103918 ) ) ;
#12532 = CARTESIAN_POINT ( 'NONE',  ( 0.05613562462218960047, 327.3245918075140821, 315.7288890211281682 ) ) ;
#12533 = ORIENTED_EDGE ( 'NONE', *, *, #10894, .F. ) ;
#12534 = CARTESIAN_POINT ( 'NONE',  ( -41.52238611146507452, 166.0448094368137504, 269.1837510020998820 ) ) ;
#12535 = VECTOR ( 'NONE', #16032, 1000.000000000000114 ) ;
#12536 = CARTESIAN_POINT ( 'NONE',  ( -89.72047535737752355, 89.01802868918773015, 51.97649104033645528 ) ) ;
#12537 = EDGE_CURVE ( 'NONE', #2301, #17537, #10839, .T. ) ;
#12538 = B_SPLINE_SURFACE_WITH_KNOTS ( 'NONE', 3, 1, ( 
 ( #19650, #1865 ),
 ( #5299, #9200 ),
 ( #10711, #5645 ),
 ( #21373, #17502 ),
 ( #3817, #14410 ),
 ( #5181, #1754 ),
 ( #3580, #7033 ),
 ( #19319, #3917 ),
 ( #20927, #17859 ),
 ( #16024, #17615 ),
 ( #8732, #17743 ),
 ( #22616, #13933 ),
 ( #7254, #1988 ),
 ( #21256, #7365 ),
 ( #14061, #8976 ),
 ( #6912, #7151 ),
 ( #12223, #12339 ),
 ( #2197, #12680 ),
 ( #10938, #8859 ),
 ( #15908, #19207 ),
 ( #261, #17961 ),
 ( #152, #3690 ),
 ( #14178, #3477 ),
 ( #14283, #5524 ),
 ( #21155, #5403 ),
 ( #21046, #10491 ),
 ( #2095, #12440 ),
 ( #19429, #15786 ),
 ( #12555, #19549 ),
 ( #372, #26 ),
 ( #10836, #9080 ),
 ( #16131, #16704 ),
 ( #16468, #4142 ),
 ( #21585, #12779 ),
 ( #14523, #11279 ),
 ( #18402, #838 ) ),
 .UNSPECIFIED., .F., .F., .F.,
 ( 4, 3, 2, 2, 2, 2, 2, 2, 2, 2, 2, 2, 2, 2, 2, 3, 4 ),
 ( 2, 2 ),
 ( -0.01000000000000000021, 0.000000000000000000, 0.1250000000000000278, 0.1875000000000000555, 0.2500000000000000555, 0.3125000000000000555, 0.3750000000000001110, 0.4375000000000001110, 0.5000000000000001110, 0.5625000000000001110, 0.6250000000000001110, 0.6875000000000001110, 0.7500000000000002220, 0.8125000000000002220, 0.8750000000000002220, 1.000000000000000000, 1.010000000000000009 ),
 ( 0.000000000000000000, 1.000000000000000000 ),
 .UNSPECIFIED. ) ;
#12539 =( GEOMETRIC_REPRESENTATION_CONTEXT ( 3 ) GLOBAL_UNCERTAINTY_ASSIGNED_CONTEXT ( ( #22522 ) ) GLOBAL_UNIT_ASSIGNED_CONTEXT ( ( #5775, #631, #14664 ) ) REPRESENTATION_CONTEXT ( 'NONE', 'WORKASPACE' ) );
#12540 = AXIS2_PLACEMENT_3D ( 'NONE', #19741, #18505, #7820 ) ;
#12542 = ORIENTED_EDGE ( 'NONE', *, *, #3461, .T. ) ;
#12541 = ORIENTED_EDGE ( 'NONE', *, *, #2912, .T. ) ;
#12543 = ORIENTED_EDGE ( 'NONE', *, *, #1920, .T. ) ;
#12544 = CARTESIAN_POINT ( 'NONE',  ( -65.60787997720018438, 111.9218655255082382, -46.61047501217030486 ) ) ;
#12545 = VECTOR ( 'NONE', #8456, 999.9999999999998863 ) ;
#12546 = DIRECTION ( 'NONE',  ( 0.4654428868037193689, 0.8850574712643738406, -0.006015952371159188211 ) ) ;
#12547 = DIRECTION ( 'NONE',  ( -0.9770372205688160339, 0.2127605332646583802, 0.01145535281434409587 ) ) ;
#12548 = CARTESIAN_POINT ( 'NONE',  ( 0.000000000000000000, 37.00000000000000711, 0.000000000000000000 ) ) ;
#12549 = VERTEX_POINT ( 'NONE', #7154 ) ;
#12550 = DIRECTION ( 'NONE',  ( 2.025474946048326158E-22, -1.000000000000000000, 1.876735158486679638E-22 ) ) ;
#12551 = EDGE_LOOP ( 'NONE', ( #20533, #18325, #20012, #8770, #21821, #3316 ) ) ;
#12552 = DIRECTION ( 'NONE',  ( 0.01292394549866734098, 0.005513023399720419666, 0.9999012842304692006 ) ) ;
#12553 = CARTESIAN_POINT ( 'NONE',  ( -41.34578887370003031, 158.5893797366368290, 277.2233642640256903 ) ) ;
#12554 = CARTESIAN_POINT ( 'NONE',  ( -110.3526887502520992, 77.12912189496645965, -26.57600582461530081 ) ) ;
#12555 = CARTESIAN_POINT ( 'NONE',  ( -25.05452705409702574, 324.4228452382362775, 308.2681417827414521 ) ) ;
#12556 = AXIS2_PLACEMENT_3D ( 'NONE', #11964, #18946, #17132 ) ;
#12557 = AXIS2_PLACEMENT_3D ( 'NONE', #17105, #1367, #8344 ) ;
#12558 = ORIENTED_EDGE ( 'NONE', *, *, #17126, .T. ) ;
#12559 = CARTESIAN_POINT ( 'NONE',  ( -105.4334892372614121, 77.28905753105595977, 31.36525700924959636 ) ) ;
#12560 = CARTESIAN_POINT ( 'NONE',  ( -39.75239154531121955, 107.1767517790489705, 71.78158818304505928 ) ) ;
#12561 = DIRECTION ( 'NONE',  ( 0.8981428216242033358, -0.000000000000000000, 0.4397038457472425277 ) ) ;
#12562 = CARTESIAN_POINT ( 'NONE',  ( -41.22219898879972533, 106.9149828242082947, 60.44841535108972153 ) ) ;
#12563 = EDGE_LOOP ( 'NONE', ( #17380, #18978, #15565, #9882 ) ) ;
#12564 = VERTEX_POINT ( 'NONE', #22316 ) ;
#12565 = AXIS2_PLACEMENT_3D ( 'NONE', #3907, #14169, #21145 ) ;
#12566 = CYLINDRICAL_SURFACE ( 'NONE', #19123, 4.000000000000006217 ) ;
#12567 = ORIENTED_EDGE ( 'NONE', *, *, #18216, .F. ) ;
#12568 = ORIENTED_EDGE ( 'NONE', *, *, #12796, .F. ) ;
#12569 = ORIENTED_EDGE ( 'NONE', *, *, #14699, .F. ) ;
#12570 = FACE_OUTER_BOUND ( 'NONE', #269, .T. ) ;
#12571 = ORIENTED_EDGE ( 'NONE', *, *, #8498, .T. ) ;
#12572 = TOROIDAL_SURFACE ( 'NONE', #18110, 20.50000000000000355, 2.000000000000000000 ) ;
#12573 = EDGE_CURVE ( 'NONE', #6559, #883, #11032, .T. ) ;
#12574 = ORIENTED_EDGE ( 'NONE', *, *, #16284, .T. ) ;
#12575 = CONICAL_SURFACE ( 'NONE', #13672, 9.000000000000001776, 1.047197551196594301 ) ;
#12576 = CIRCLE ( 'NONE', #22329, 7.921742784567035400 ) ;
#12577 = FACE_OUTER_BOUND ( 'NONE', #12976, .T. ) ;
#12578 = DIRECTION ( 'NONE',  ( 0.2317097747526812579, -0.9727820773532223075, 0.002368599673008277024 ) ) ;
#12579 = CARTESIAN_POINT ( 'NONE',  ( 4.182528737366220106, 166.7840834110302808, 323.5943587238651276 ) ) ;
#12580 = DIRECTION ( 'NONE',  ( 0.009138748381789079875, 0.7071067811865487940, 0.7070477234798316912 ) ) ;
#12581 = CARTESIAN_POINT ( 'NONE',  ( -38.86688258710752564, 95.50318961173329058, 82.87093702155239328 ) ) ;
#12582 = CIRCLE ( 'NONE', #2678, 4.200000000000005507 ) ;
#12583 = EDGE_LOOP ( 'NONE', ( #5464, #18386, #20227, #12764 ) ) ;
#12584 = FILL_AREA_STYLE ('',( #3497 ) ) ;
#12585 = CARTESIAN_POINT ( 'NONE',  ( 79.09341253102171265, 75.20311826365394836, -7.232296047367152703 ) ) ;
#12586 = CARTESIAN_POINT ( 'NONE',  ( 19.81846420101658879, 182.7288148374562411, 310.4831695857175760 ) ) ;
#12587 = DIRECTION ( 'NONE',  ( 0.01292414190464117631, 5.551059884324762197E-17, 0.9999164797902017066 ) ) ;
#12588 = EDGE_CURVE ( 'NONE', #22140, #16183, #9678, .T. ) ;
#12589 = PLANE ( 'NONE',  #9169 ) ;
#12590 = VERTEX_POINT ( 'NONE', #720 ) ;
#12591 = AXIS2_PLACEMENT_3D ( 'NONE', #8814, #15864, #109 ) ;
#12592 = VECTOR ( 'NONE', #1119, 1000.000000000000000 ) ;
#12593 = ADVANCED_FACE ( 'NONE', ( #11391 ), #11467, .T. ) ;
#12594 = CARTESIAN_POINT ( 'NONE',  ( -39.06279898716250187, 108.3240682923980245, 72.76796811295301382 ) ) ;
#12595 = CARTESIAN_POINT ( 'NONE',  ( -21.30129866354426582, 189.4444907833431273, -100.5497760856508478 ) ) ;
#12596 = ORIENTED_EDGE ( 'NONE', *, *, #18209, .T. ) ;
#12597 = CARTESIAN_POINT ( 'NONE',  ( -92.62880990220969579, 79.84869560962759749, -28.85690742247488672 ) ) ;
#12598 = VERTEX_POINT ( 'NONE', #21590 ) ;
#12599 = EDGE_CURVE ( 'NONE', #21368, #9437, #12216, .T. ) ;
#12600 = ADVANCED_FACE ( 'NONE', ( #14636 ), #10373, .F. ) ;
#12601 = EDGE_LOOP ( 'NONE', ( #11617, #4924, #8409, #14406, #22521, #9874 ) ) ;
#12602 = CARTESIAN_POINT ( 'NONE',  ( -8.312614011469616315, 81.99999999999998579, -95.45924547291811280 ) ) ;
#12603 = EDGE_CURVE ( 'NONE', #14141, #5939, #1564, .T. ) ;
#12604 = SURFACE_SIDE_STYLE ('',( #5571 ) ) ;
#12605 = CIRCLE ( 'NONE', #1252, 2.000000000000000888 ) ;
#12606 = ADVANCED_FACE ( 'NONE', ( #13130 ), #11057, .F. ) ;
#12607 = DIRECTION ( 'NONE',  ( 2.025474946048326158E-22, -1.000000000000000000, 1.876735158486678933E-22 ) ) ;
#12608 = FACE_OUTER_BOUND ( 'NONE', #5734, .T. ) ;
#12609 = ORIENTED_EDGE ( 'NONE', *, *, #14925, .F. ) ;
#12610 = CARTESIAN_POINT ( 'NONE',  ( 12.18522217402714070, 187.7091244767421188, 322.9747985970192872 ) ) ;
#12611 = ORIENTED_EDGE ( 'NONE', *, *, #13218, .F. ) ;
#12612 = ORIENTED_EDGE ( 'NONE', *, *, #5705, .F. ) ;
#12613 = PLANE ( 'NONE',  #9329 ) ;
#12614 = ADVANCED_FACE ( 'NONE', ( #5871, #7837, #12904 ), #21708, .F. ) ;
#12615 = CARTESIAN_POINT ( 'NONE',  ( 67.26198047107926925, 70.17996908938924605, -87.03937574298602442 ) ) ;
#12616 =( LENGTH_UNIT ( ) NAMED_UNIT ( * ) SI_UNIT ( .MILLI., .METRE. ) );
#12617 = CARTESIAN_POINT ( 'NONE',  ( -89.97519728687143470, 79.29963411167480558, 29.42247391813824109 ) ) ;
#12618 = FACE_OUTER_BOUND ( 'NONE', #5673, .T. ) ;
#12619 = AXIS2_PLACEMENT_3D ( 'NONE', #16276, #18430, #19901 ) ;
#12620 = ADVANCED_FACE ( 'NONE', ( #4365 ), #5995, .T. ) ;
#12621 = ORIENTED_EDGE ( 'NONE', *, *, #22387, .T. ) ;
#12622 = CARTESIAN_POINT ( 'NONE',  ( -15.07023257787665749, 179.7582508136519266, 316.0339885398511797 ) ) ;
#12623 = ADVANCED_FACE ( 'NONE', ( #13032 ), #2200, .F. ) ;
#12624 = ORIENTED_EDGE ( 'NONE', *, *, #7843, .T. ) ;
#12625 = ADVANCED_FACE ( 'NONE', ( #21488 ), #19992, .T. ) ;
#12626 = VERTEX_POINT ( 'NONE', #9556 ) ;
#12627 = DIRECTION ( 'NONE',  ( -7.125109674158749138E-05, 0.9999848031710253382, -0.005512562950850162860 ) ) ;
#12628 = CARTESIAN_POINT ( 'NONE',  ( 19.29271048405903244, 168.4538167080974063, 309.1579687774811305 ) ) ;
#12629 = CARTESIAN_POINT ( 'NONE',  ( -15.49848325445370989, 177.8265085296330028, 315.8457734436829583 ) ) ;
#12630 = AXIS2_PLACEMENT_3D ( 'NONE', #16488, #14776, #21728 ) ;
#12631 = ORIENTED_EDGE ( 'NONE', *, *, #21192, .T. ) ;
#12632 = LINE ( 'NONE', #21328, #15426 ) ;
#12633 = ORIENTED_EDGE ( 'NONE', *, *, #11514, .F. ) ;
#12634 = CARTESIAN_POINT ( 'NONE',  ( 71.61338682171094661, 92.58578643762700722, 83.49564556265194426 ) ) ;
#12635 = ADVANCED_FACE ( 'NONE', ( #4258 ), #9202, .T. ) ;
#12636 = AXIS2_PLACEMENT_3D ( 'NONE', #9198, #19871, #5747 ) ;
#12637 = CARTESIAN_POINT ( 'NONE',  ( -162.0000000000000000, 1.999999999999998224, 53.76161406891260697 ) ) ;
#12638 = CARTESIAN_POINT ( 'NONE',  ( -9.064738643541179641, 105.7168211570308500, 130.3284763332909222 ) ) ;
#12639 = DIRECTION ( 'NONE',  ( 0.9999164797902017066, -6.938893703802208150E-15, -0.01292414190464825571 ) ) ;
#12640 = VERTEX_POINT ( 'NONE', #18404 ) ;
#12641 = AXIS2_PLACEMENT_3D ( 'NONE', #8910, #15960, #5456 ) ;
#12642 = ORIENTED_EDGE ( 'NONE', *, *, #22626, .F. ) ;
#12643 = CYLINDRICAL_SURFACE ( 'NONE', #882, 3.099999999999998757 ) ;
#12644 = CIRCLE ( 'NONE', #7113, 2.000000000000001332 ) ;
#12645 = FACE_OUTER_BOUND ( 'NONE', #2274, .T. ) ;
#12646 = CARTESIAN_POINT ( 'NONE',  ( -48.56578001921132426, 94.99786382055523859, -43.46314047150291060 ) ) ;
#12647 = EDGE_LOOP ( 'NONE', ( #14802, #3835, #9206, #21142, #13479 ) ) ;
#12648 = DIRECTION ( 'NONE',  ( -0.9909299940865187173, 0.1338359446631173233, 0.01207007604876291287 ) ) ;
#12649 =( NAMED_UNIT ( * ) SI_UNIT ( $, .STERADIAN. ) SOLID_ANGLE_UNIT ( ) );
#12650 = DIRECTION ( 'NONE',  ( 0.000000000000000000, 0.000000000000000000, -1.000000000000000000 ) ) ;
#12651 = DIRECTION ( 'NONE',  ( -0.01292394549866637994, -0.005513023399719273882, -0.9999012842304692006 ) ) ;
#12652 = DIRECTION ( 'NONE',  ( -0.01035335185279007662, -0.005513005182356926943, -0.9999312050732648283 ) ) ;
#12653 = ORIENTED_EDGE ( 'NONE', *, *, #5726, .T. ) ;
#12654 = ORIENTED_EDGE ( 'NONE', *, *, #15558, .F. ) ;
#12655 = EDGE_CURVE ( 'NONE', #22152, #10082, #18805, .T. ) ;
#12656 = CARTESIAN_POINT ( 'NONE',  ( 16.20940818329404820, 145.7950971976291612, 277.5076651938596797 ) ) ;
#12657 = CIRCLE ( 'NONE', #2003, 10.00000000000000888 ) ;
#12658 = CARTESIAN_POINT ( 'NONE',  ( 41.09169241204631362, 95.99012513974443550, 84.20368898025243709 ) ) ;
#12659 = ORIENTED_EDGE ( 'NONE', *, *, #1239, .F. ) ;
#12660 = VECTOR ( 'NONE', #1485, 1000.000000000000114 ) ;
#12661 = CARTESIAN_POINT ( 'NONE',  ( -38.68617183816869698, 163.9153776386440882, 273.1592279730091377 ) ) ;
#12662 = CARTESIAN_POINT ( 'NONE',  ( -89.92919990131169072, 88.83226839477106296, 52.34107143949843532 ) ) ;
#12663 = EDGE_CURVE ( 'NONE', #20978, #5358, #492, .T. ) ;
#12664 = PRODUCT_CONTEXT ( 'NONE', #22277, 'mechanical' ) ;
#12665 = ORIENTED_EDGE ( 'NONE', *, *, #22384, .T. ) ;
#12666 =( REPRESENTATION_RELATIONSHIP ('NONE','NONE', #11808, #21889 ) REPRESENTATION_RELATIONSHIP_WITH_TRANSFORMATION ( #12296 )SHAPE_REPRESENTATION_RELATIONSHIP( ) );
#12667 = ORIENTED_EDGE ( 'NONE', *, *, #11904, .T. ) ;
#12668 = CARTESIAN_POINT ( 'NONE',  ( -13.99926948760909795, 325.7454604562529425, 322.7258004511344325 ) ) ;
#12669 = LINE ( 'NONE', #7479, #8870 ) ;
#12670 = VERTEX_POINT ( 'NONE', #9327 ) ;
#12671 = PRESENTATION_LAYER_ASSIGNMENT (  '', '', ( #18876 ) ) ;
#12672 = DIRECTION ( 'NONE',  ( -0.01292394549866740169, -0.005513023399719838534, -0.9999012842304693116 ) ) ;
#12673 = FACE_OUTER_BOUND ( 'NONE', #4034, .T. ) ;
#12674 = ORIENTED_EDGE ( 'NONE', *, *, #15406, .T. ) ;
#12675 = CARTESIAN_POINT ( 'NONE',  ( -40.58111162538312300, 119.0295134562300063, 187.4227113448806961 ) ) ;
#12676 = ORIENTED_EDGE ( 'NONE', *, *, #8358, .F. ) ;
#12677 = FACE_OUTER_BOUND ( 'NONE', #18969, .T. ) ;
#12678 = CARTESIAN_POINT ( 'NONE',  ( -14.85563907056677913, 177.4876913356084174, 88.64044390550773755 ) ) ;
#12679 = CARTESIAN_POINT ( 'NONE',  ( -78.90025544361535026, 75.13007332810630601, -3.950326719918461293 ) ) ;
#12680 = CARTESIAN_POINT ( 'NONE',  ( -13.80923234909357333, 164.6932440001694431, 315.3391977597048594 ) ) ;
#12681 = DIRECTION ( 'NONE',  ( 0.01292394549866739996, 0.005513023399721131770, 0.9999012842304692006 ) ) ;
#12682 = ADVANCED_FACE ( 'NONE', ( #15535, #4815, #15206, #17133 ), #3108, .F. ) ;
#12683 = DIRECTION ( 'NONE',  ( -7.125109674118361251E-05, 0.9999848031710253382, -0.005512562950849477644 ) ) ;
#12684 = CARTESIAN_POINT ( 'NONE',  ( 161.9999999999998579, 20.00000000000000000, -10.00000000000224176 ) ) ;
#12685 = EDGE_CURVE ( 'NONE', #17346, #9463, #20342, .T. ) ;
#12686 = CYLINDRICAL_SURFACE ( 'NONE', #8442, 110.0000000000000000 ) ;
#12687 = ORIENTED_EDGE ( 'NONE', *, *, #12573, .F. ) ;
#12688 = DIRECTION ( 'NONE',  ( 0.01035335185279151644, 0.005513005182356664133, 0.9999312050732649393 ) ) ;
#12689 = ORIENTED_EDGE ( 'NONE', *, *, #7852, .T. ) ;
#12690 = VECTOR ( 'NONE', #4568, 1000.000000000000000 ) ;
#12691 = ORIENTED_EDGE ( 'NONE', *, *, #10829, .F. ) ;
#12692 = CARTESIAN_POINT ( 'NONE',  ( -80.26018450689494443, 75.13699351169597662, 6.137806644758510011 ) ) ;
#12693 = DIRECTION ( 'NONE',  ( 2.025474946048326158E-22, -1.000000000000000000, 1.876735158486679638E-22 ) ) ;
#12694 = ORIENTED_EDGE ( 'NONE', *, *, #22523, .F. ) ;
#12695 = DIRECTION ( 'NONE',  ( 0.01292414190464174703, 0.000000000000000000, 0.9999164797902015955 ) ) ;
#12696 = PLANE ( 'NONE',  #20857 ) ;
#12697 = CARTESIAN_POINT ( 'NONE',  ( 5.806620212786449464, 70.35526451184087193, -96.66860143004628014 ) ) ;
#12698 = B_SPLINE_CURVE_WITH_KNOTS ( 'NONE', 3,
 ( #11479, #20070, #9757, #18364, #6307, #4454, #13211, #13332, #20518, #4564, #2634, #13436, #11696, #17003 ),
 .UNSPECIFIED., .F., .F.,
 ( 4, 2, 2, 2, 2, 2, 4 ),
 ( 1.387778780781445676E-17, 0.0003920573607328231873, 0.0007841147214656324967, 0.001176172082198441698, 0.001568229442931251116, 0.002352344164396850002, 0.003136458885862449322 ),
 .UNSPECIFIED. ) ;
#12699 = DIRECTION ( 'NONE',  ( 0.9999164797902015955, 0.000000000000000000, -0.01292414190463754553 ) ) ;
#12700 = CARTESIAN_POINT ( 'NONE',  ( 27.99766143412564290, 170.0000000000008242, -0.3618759733291194713 ) ) ;
#12701 = AXIS2_PLACEMENT_3D ( 'NONE', #13457, #2982, #20088 ) ;
#12702 = CARTESIAN_POINT ( 'NONE',  ( 42.04378466868516995, 168.6907664596096765, 34.06594930769865925 ) ) ;
#12703 = CARTESIAN_POINT ( 'NONE',  ( 16.78432341940586880, 185.2449657461795027, 308.8478038024924217 ) ) ;
#12704 = CARTESIAN_POINT ( 'NONE',  ( 89.24560213809748177, 80.14548850073731501, 29.69112557292140053 ) ) ;
#12705 = EDGE_CURVE ( 'NONE', #19209, #6360, #2879, .T. ) ;
#12706 = DIRECTION ( 'NONE',  ( 0.9999164797902017066, 0.000000000000000000, -0.01292414190464177826 ) ) ;
#12707 = ORIENTED_EDGE ( 'NONE', *, *, #10299, .T. ) ;
#12708 = SHAPE_REPRESENTATION_RELATIONSHIP ( 'NONE' , 'NONE' ,  #2270, #19482 ) ;
#12709 = DIRECTION ( 'NONE',  ( 0.9999164797902017066, 0.000000000000000000, -0.01292414190463832269 ) ) ;
#12710 = ORIENTED_EDGE ( 'NONE', *, *, #9973, .F. ) ;
#12711 = CARTESIAN_POINT ( 'NONE',  ( -91.32446103601363063, 78.00118640252709667, -30.19495016275356747 ) ) ;
#12712 = ORIENTED_EDGE ( 'NONE', *, *, #21292, .T. ) ;
#12713 = ORIENTED_EDGE ( 'NONE', *, *, #17873, .F. ) ;
#12714 = LINE ( 'NONE', #19682, #13971 ) ;
#12715 = ADVANCED_FACE ( 'NONE', ( #18618 ), #11856, .F. ) ;
#12716 =( LENGTH_UNIT ( ) NAMED_UNIT ( * ) SI_UNIT ( .MILLI., .METRE. ) );
#12717 = PRODUCT_DEFINITION_CONTEXT ( 'detailed design', #1916, 'design' ) ;
#12718 = DIRECTION ( 'NONE',  ( -5.440186201345738641E-18, -1.000000000000000000, -1.334940939666364181E-17 ) ) ;
#12719 = CARTESIAN_POINT ( 'NONE',  ( 76.92953810531172110, 75.15462563255036343, 4.428914867104452036 ) ) ;
#12720 = DIRECTION ( 'NONE',  ( 0.9999164797902017066, 2.001050586450178931E-22, -0.01292414190464131508 ) ) ;
#12721 = LINE ( 'NONE', #7296, #21733 ) ;
#12722 = VERTEX_POINT ( 'NONE', #11731 ) ;
#12723 = CARTESIAN_POINT ( 'NONE',  ( 12.41521462045219693, 188.2702244292405283, 320.9524563331297031 ) ) ;
#12724 = DIRECTION ( 'NONE',  ( 1.000000000000000000, 0.000000000000000000, 0.000000000000000000 ) ) ;
#12725 = CARTESIAN_POINT ( 'NONE',  ( -55.98629706596215527, 114.1919480473872852, 162.6802715674982664 ) ) ;
#12726 = CARTESIAN_POINT ( 'NONE',  ( 66.07231611197045140, 94.48610424851698042, 82.54302267323386388 ) ) ;
#12727 = CARTESIAN_POINT ( 'NONE',  ( -9.065023647928146744, 109.7167603697149474, 130.3064260814875013 ) ) ;
#12728 = CARTESIAN_POINT ( 'NONE',  ( -91.14374963600238289, 79.10773180776112667, 28.81380175419842615 ) ) ;
#12729 = EDGE_LOOP ( 'NONE', ( #8040, #19254, #1729, #7477 ) ) ;
#12730 = ADVANCED_FACE ( 'NONE', ( #4933 ), #16914, .F. ) ;
#12731 = DIRECTION ( 'NONE',  ( 2.025474946048326158E-22, -1.000000000000000000, 1.876735158486679638E-22 ) ) ;
#12732 = ADVANCED_FACE ( 'NONE', ( #15084 ), #4599, .F. ) ;
#12733 = CARTESIAN_POINT ( 'NONE',  ( -56.11381622223437660, 118.5884715842524315, 107.6180086640604543 ) ) ;
#12734 = CARTESIAN_POINT ( 'NONE',  ( -14.18436105576317985, 179.8295574832275463, 320.1833246747981434 ) ) ;
#12735 = VERTEX_POINT ( 'NONE', #20443 ) ;
#12736 = FACE_OUTER_BOUND ( 'NONE', #9266, .T. ) ;
#12737 = ORIENTED_EDGE ( 'NONE', *, *, #6613, .T. ) ;
#12738 = CARTESIAN_POINT ( 'NONE',  ( -10.78894434267867197, 113.7357082962960817, 133.7548551926877280 ) ) ;
#12739 = EDGE_CURVE ( 'NONE', #13713, #21368, #16645, .T. ) ;
#12740 = EDGE_CURVE ( 'NONE', #12590, #5091, #9789, .T. ) ;
#12741 = ORIENTED_EDGE ( 'NONE', *, *, #10784, .F. ) ;
#12742 = DIRECTION ( 'NONE',  ( -7.125109674161231961E-05, 0.9999848031710252272, -0.005512562950850142043 ) ) ;
#12743 = ADVANCED_FACE ( 'NONE', ( #18727 ), #13363, .T. ) ;
#12744 = CARTESIAN_POINT ( 'NONE',  ( 50.25511493332505353, 111.2913824189418364, -47.87582765672370044 ) ) ;
#12745 = ORIENTED_EDGE ( 'NONE', *, *, #5707, .F. ) ;
#12746 = ORIENTED_EDGE ( 'NONE', *, *, #20555, .F. ) ;
#12747 = CARTESIAN_POINT ( 'NONE',  ( 42.91324393340197219, 106.8060942374655156, 70.38454212103849272 ) ) ;
#12748 = CARTESIAN_POINT ( 'NONE',  ( 50.76788212671708322, 169.4762627770265340, -95.66267738093596051 ) ) ;
#12749 = ORIENTED_EDGE ( 'NONE', *, *, #6764, .F. ) ;
#12750 = CARTESIAN_POINT ( 'NONE',  ( -41.94323954856972136, 174.9483409995870886, 5.436613131876677940 ) ) ;
#12751 = VERTEX_POINT ( 'NONE', #4696 ) ;
#12752 = DIRECTION ( 'NONE',  ( 0.000000000000000000, -1.000000000000000000, -0.000000000000000000 ) ) ;
#12753 = DIRECTION ( 'NONE',  ( 0.000000000000000000, -0.000000000000000000, 1.000000000000000000 ) ) ;
#12754 = CARTESIAN_POINT ( 'NONE',  ( -55.33808647217894361, 114.8068154851947753, 167.6347561330238420 ) ) ;
#12755 = CARTESIAN_POINT ( 'NONE',  ( -20.14358671158747072, 88.61365832079873428, 77.93650841479222890 ) ) ;
#12756 = EDGE_CURVE ( 'NONE', #21685, #2070, #124, .T. ) ;
#12757 = CARTESIAN_POINT ( 'NONE',  ( 3.755496156877637492, 174.6347345924375531, 296.5539275290220189 ) ) ;
#12758 = ADVANCED_FACE ( 'NONE', ( #22264 ), #15424, .F. ) ;
#12759 = CARTESIAN_POINT ( 'NONE',  ( 40.65822637310716203, 69.99999999999998579, 84.25167897319536792 ) ) ;
#12760 = ORIENTED_EDGE ( 'NONE', *, *, #2424, .T. ) ;
#12761 = CARTESIAN_POINT ( 'NONE',  ( 41.12451612944703783, 107.6443775000873160, 71.14585205175409044 ) ) ;
#12762 = CARTESIAN_POINT ( 'NONE',  ( -88.18706637290516426, 88.71869973106716145, 50.32066939225187241 ) ) ;
#12763 = SHAPE_DEFINITION_REPRESENTATION ( #7204, #15770 ) ;
#12764 = ORIENTED_EDGE ( 'NONE', *, *, #2315, .F. ) ;
#12765 = CARTESIAN_POINT ( 'NONE',  ( -90.83733885584940992, 70.37256007341385100, 62.03708646394351689 ) ) ;
#12766 = ADVANCED_FACE ( 'NONE', ( #22373 ), #17242, .F. ) ;
#12767 = ORIENTED_EDGE ( 'NONE', *, *, #16295, .T. ) ;
#12768 = CYLINDRICAL_SURFACE ( 'NONE', #11439, 2.000000000000004441 ) ;
#12769 = CARTESIAN_POINT ( 'NONE',  ( -90.00000000000000000, 0.000000000000000000, 10.99999999999999289 ) ) ;
#12770 = ORIENTED_EDGE ( 'NONE', *, *, #5912, .T. ) ;
#12771 = CARTESIAN_POINT ( 'NONE',  ( -106.1801133998812929, 71.34284122058934940, -28.73649967668641381 ) ) ;
#12772 = AXIS2_PLACEMENT_3D ( 'NONE', #5376, #3554, #17360 ) ;
#12773 = VERTEX_POINT ( 'NONE', #17034 ) ;
#12774 = CARTESIAN_POINT ( 'NONE',  ( -47.66114072508762689, 168.8134312302532862, 57.47692565324432934 ) ) ;
#12775 = ORIENTED_EDGE ( 'NONE', *, *, #9347, .F. ) ;
#12776 = CARTESIAN_POINT ( 'NONE',  ( -57.08936890124425645, 114.5600912807551879, 172.9077466791229654 ) ) ;
#12777 = DIRECTION ( 'NONE',  ( 0.009188991635466048358, -0.7031977391749438810, 0.7109349492407661675 ) ) ;
#12778 = CARTESIAN_POINT ( 'NONE',  ( -10.85567112094788200, 105.6999953372425551, 127.2994028633183348 ) ) ;
#12779 = CARTESIAN_POINT ( 'NONE',  ( -7.896211107215091118, 165.3408590920663244, 308.2534447097586963 ) ) ;
#12780 = CARTESIAN_POINT ( 'NONE',  ( -10.02117361870881851, 187.8727420016839176, 308.1601407300097435 ) ) ;
#12781 = ADVANCED_FACE ( 'NONE', ( #13574 ), #8489, .F. ) ;
#12782 = DIRECTION ( 'NONE',  ( 0.1296504907605104673, 0.005475273188900901117, 0.9915446392518421082 ) ) ;
#12783 = DIRECTION ( 'NONE',  ( 0.01292394549866695240, 0.005513023399711377420, 0.9999012842304693116 ) ) ;
#12784 = CARTESIAN_POINT ( 'NONE',  ( 40.58925859504437739, 106.0715746962035695, 92.05426835618892767 ) ) ;
#12785 = AXIS2_PLACEMENT_3D ( 'NONE', #11736, #2883, #8495 ) ;
#12786 = ORIENTED_EDGE ( 'NONE', *, *, #20003, .T. ) ;
#12787 = CARTESIAN_POINT ( 'NONE',  ( -41.00000899811524846, 169.5540992312279229, 273.1580453575298293 ) ) ;
#12788 = ORIENTED_EDGE ( 'NONE', *, *, #13051, .T. ) ;
#12789 = ORIENTED_EDGE ( 'NONE', *, *, #21191, .T. ) ;
#12790 = CARTESIAN_POINT ( 'NONE',  ( -105.1274178938603825, 70.25451017443430146, 32.37651503794364771 ) ) ;
#12791 = PRESENTATION_LAYER_ASSIGNMENT (  '', '', ( #21196 ) ) ;
#12792 = CARTESIAN_POINT ( 'NONE',  ( -88.16274635857531905, 88.18390162297423274, 52.97334896370593782 ) ) ;
#12793 = EDGE_LOOP ( 'NONE', ( #10147, #1003, #12809, #5823 ) ) ;
#12795 = ORIENTED_EDGE ( 'NONE', *, *, #5154, .T. ) ;
#12794 = ORIENTED_EDGE ( 'NONE', *, *, #15823, .F. ) ;
#12796 = EDGE_CURVE ( 'NONE', #5654, #12220, #3339, .T. ) ;
#12797 = EDGE_CURVE ( 'NONE', #4876, #13067, #17591, .T. ) ;
#12798 = CARTESIAN_POINT ( 'NONE',  ( 39.62116574264821622, 95.66828032177839702, -43.44368198931868363 ) ) ;
#12799 = DIRECTION ( 'NONE',  ( 0.01292394549866737567, 0.005513023399721124831, 0.9999012842304693116 ) ) ;
#12800 = AXIS2_PLACEMENT_3D ( 'NONE', #11210, #5908, #14906 ) ;
#12801 = CARTESIAN_POINT ( 'NONE',  ( 0.000000000000000000, 23.00000000000000000, 0.000000000000000000 ) ) ;
#12802 = CIRCLE ( 'NONE', #16842, 6.000000000000000888 ) ;
#12803 = MECHANICAL_DESIGN_GEOMETRIC_PRESENTATION_REPRESENTATION (  '', ( #9496 ), #22650 ) ;
#12804 = CARTESIAN_POINT ( 'NONE',  ( 146.4999999999998579, 18.00000000000000355, 10.00000000000198952 ) ) ;
#12805 = CYLINDRICAL_SURFACE ( 'NONE', #20656, 2.000000000000004885 ) ;
#12806 = CARTESIAN_POINT ( 'NONE',  ( 20.11979018982224687, 182.4391765495445838, 311.2061076290632968 ) ) ;
#12807 = CARTESIAN_POINT ( 'NONE',  ( -146.5000000000000000, 1.999999999999998224, -9.999999999999980460 ) ) ;
#12808 = CARTESIAN_POINT ( 'NONE',  ( 55.40268456415110165, 20.00000000000000000, 113.1659955246503415 ) ) ;
#12809 = ORIENTED_EDGE ( 'NONE', *, *, #13993, .T. ) ;
#12810 =( BOUNDED_SURFACE ( )  B_SPLINE_SURFACE ( 3, 2, ( 
 ( #4711, #10029, #860 ),
 ( #11409, #16607, #7853 ),
 ( #20110, #18533, #14986 ),
 ( #2895, #4381, #18419 ) ),
 .UNSPECIFIED., .F., .F., .T. ) 
 B_SPLINE_SURFACE_WITH_KNOTS ( ( 4, 4 ),
 ( 3, 3 ),
 ( 0.07609981584028600865, 0.08941542774493665968 ),
 ( 0.000000000000000000, 1.000000000000000000 ),
 .UNSPECIFIED. ) 
 GEOMETRIC_REPRESENTATION_ITEM ( )  RATIONAL_B_SPLINE_SURFACE ( (
 ( 1.000000000000000000, 0.6989529655644959316, 1.000000000000000000),
 ( 1.000000000000000000, 0.6987865376935388229, 1.000000000000000000),
 ( 1.000000000000000000, 0.6986099777012620970, 1.000000000000000000),
 ( 1.000000000000000000, 0.6984211671062240390, 1.000000000000000000) ) ) 
 REPRESENTATION_ITEM ( '' )  SURFACE ( )  );
#12811 = CARTESIAN_POINT ( 'NONE',  ( 394.6585245357460963, 69.99999999999997158, -112.1099862245463896 ) ) ;
#12812 = VERTEX_POINT ( 'NONE', #8836 ) ;
#12813 = CARTESIAN_POINT ( 'NONE',  ( -14.93612093091044102, 185.1121758471145142, 276.7357782268812798 ) ) ;
#12814 = CIRCLE ( 'NONE', #22318, 2.000000000000001332 ) ;
#12815 = ORIENTED_EDGE ( 'NONE', *, *, #5330, .T. ) ;
#12816 = B_SPLINE_CURVE_WITH_KNOTS ( 'NONE', 3,
 ( #3761, #5463, #207, #5589 ),
 .UNSPECIFIED., .F., .F.,
 ( 4, 4 ),
 ( 2.380735204150486297E-07, 0.002921158035944664000 ),
 .UNSPECIFIED. ) ;
#12817 = CARTESIAN_POINT ( 'NONE',  ( -9.127842323083935838, 105.6832193904443784, 124.2338956383693613 ) ) ;
#12818 = AXIS2_PLACEMENT_3D ( 'NONE', #1711, #3301, #12294 ) ;
#12819 = EDGE_CURVE ( 'NONE', #12670, #20506, #8549, .T. ) ;
#12820 = CARTESIAN_POINT ( 'NONE',  ( -0.003538370294055813436, 69.99999999999998579, -98.91746206376724615 ) ) ;
#12821 = CARTESIAN_POINT ( 'NONE',  ( 26.28163433660693471, 55.00725983767637928, -133.1276554916787518 ) ) ;
#12822 = LINE ( 'NONE', #18003, #13670 ) ;
#12823 = CARTESIAN_POINT ( 'NONE',  ( -64.99457118636308905, 169.9999999999999716, 0.8400692238016759239 ) ) ;
#12824 = CARTESIAN_POINT ( 'NONE',  ( 41.22179815901248645, 127.3750215702999213, 249.0188771933985663 ) ) ;
#12825 = LINE ( 'NONE', #19804, #6375 ) ;
#12826 = ORIENTED_EDGE ( 'NONE', *, *, #17818, .T. ) ;
#12827 = DIRECTION ( 'NONE',  ( 0.2126763768167737323, 0.9770888199431678744, -0.008136134595576589509 ) ) ;
#12828 = DIRECTION ( 'NONE',  ( 0.000000000000000000, 0.000000000000000000, 1.000000000000000000 ) ) ;
#12829 = DIRECTION ( 'NONE',  ( -7.125109674403276030E-05, 0.9999848031710252272, -0.005512562950848280685 ) ) ;
#12830 = AXIS2_PLACEMENT_3D ( 'NONE', #21369, #12550, #3912 ) ;
#12831 = PLANE ( 'NONE',  #10063 ) ;
#12832 = AXIS2_PLACEMENT_3D ( 'NONE', #3152, #4866, #10166 ) ;
#12833 = DIRECTION ( 'NONE',  ( 0.01292394549866731843, 0.005513023399720594006, 0.9999012842304693116 ) ) ;
#12834 = VECTOR ( 'NONE', #12160, 1000.000000000000227 ) ;
#12836 = CARTESIAN_POINT ( 'NONE',  ( -39.39497909003006981, 69.99999999999998579, 85.51628863845817818 ) ) ;
#12835 = CARTESIAN_POINT ( 'NONE',  ( -90.42410873942375815, 78.25489917908669213, 32.91867509261335556 ) ) ;
#12837 = DIRECTION ( 'NONE',  ( 7.125109674364534776E-05, -0.9999848031710252272, 0.005512562950849704893 ) ) ;
#12838 = ORIENTED_EDGE ( 'NONE', *, *, #22653, .F. ) ;
#12839 = DIRECTION ( 'NONE',  ( -0.01292394549866738782, -0.005513023399720468239, -0.9999012842304692006 ) ) ;
#12840 = B_SPLINE_CURVE_WITH_KNOTS ( 'NONE', 3,
 ( #7571, #22613, #19837, #19721, #21344, #14603, #5830 ),
 .UNSPECIFIED., .F., .F.,
 ( 4, 3, 4 ),
 ( 0.000000000000000000, 0.005203688037432161254, 0.009927031861615774611 ),
 .UNSPECIFIED. ) ;
#12841 = DIRECTION ( 'NONE',  ( 0.000000000000000000, -1.000000000000000000, -0.000000000000000000 ) ) ;
#12842 = CARTESIAN_POINT ( 'NONE',  ( -14.34549876140896174, 179.6624466946600194, 317.9627730398437393 ) ) ;
#12843 = ORIENTED_EDGE ( 'NONE', *, *, #22012, .T. ) ;
#12844 = EDGE_LOOP ( 'NONE', ( #14532, #4760 ) ) ;
#12845 = DIRECTION ( 'NONE',  ( 0.9999164797902015955, 2.001050586450178695E-22, -0.01292414190464131335 ) ) ;
#12846 = CIRCLE ( 'NONE', #21246, 7.499999999999992006 ) ;
#12847 = EDGE_CURVE ( 'NONE', #3054, #8988, #1238, .T. ) ;
#12848 = VECTOR ( 'NONE', #1052, 1000.000000000000000 ) ;
#12849 = CARTESIAN_POINT ( 'NONE',  ( 67.23655452815148692, 145.1029152106949027, 17.86880078497820179 ) ) ;
#12850 = ADVANCED_FACE ( 'NONE', ( #15881, #127 ), #3450, .F. ) ;
#12851 = CARTESIAN_POINT ( 'NONE',  ( -1.163172771417702700, 37.00000000000000711, -89.99248318111824574 ) ) ;
#12852 = AXIS2_PLACEMENT_3D ( 'NONE', #12733, #21324, #10776 ) ;
#12853 = CARTESIAN_POINT ( 'NONE',  ( -27.99766143412566421, 170.0000000000008242, 0.3618759733308087312 ) ) ;
#12854 = ORIENTED_EDGE ( 'NONE', *, *, #17071, .F. ) ;
#12855 = ORIENTED_EDGE ( 'NONE', *, *, #5568, .F. ) ;
#12856 = CARTESIAN_POINT ( 'NONE',  ( 40.57709715711068554, 106.0996895337223265, 199.1395768038429424 ) ) ;
#12857 = EDGE_LOOP ( 'NONE', ( #17964, #2183, #13195, #15718, #9994, #17568 ) ) ;
#12858 = CARTESIAN_POINT ( 'NONE',  ( 3.238538336930941508, 174.4142136564487373, 256.5578761598032429 ) ) ;
#12859 = DIRECTION ( 'NONE',  ( 0.01035335185279143318, 0.005513005182356926943, 0.9999312050732649393 ) ) ;
#12860 = EDGE_LOOP ( 'NONE', ( #12854, #16599, #10455, #21243 ) ) ;
#12861 = CARTESIAN_POINT ( 'NONE',  ( -162.0000000000000000, 0.000000000000000000, -9.999999999999978684 ) ) ;
#12862 = CARTESIAN_POINT ( 'NONE',  ( -41.87517931370788915, 95.06543052087248213, -43.43230847621652657 ) ) ;
#12863 = CARTESIAN_POINT ( 'NONE',  ( 1.117803423002110774, 45.00000000000000000, 109.6947150755565161 ) ) ;
#12864 = AXIS2_PLACEMENT_3D ( 'NONE', #15482, #4985, #12012 ) ;
#12865 = CIRCLE ( 'NONE', #18715, 10.00000000000001421 ) ;
#12866 = EDGE_CURVE ( 'NONE', #13585, #21883, #10759, .T. ) ;
#12867 = CARTESIAN_POINT ( 'NONE',  ( 4.917494328089510702, 70.07661102881314719, -83.12797620812510502 ) ) ;
#12868 = AXIS2_PLACEMENT_3D ( 'NONE', #12328, #140, #7138 ) ;
#12869 = AXIS2_PLACEMENT_3D ( 'NONE', #2601, #9256, #14572 ) ;
#12870 = LINE ( 'NONE', #19728, #6232 ) ;
#12871 = ADVANCED_FACE ( 'NONE', ( #17480 ), #14154, .F. ) ;
#12872 = AXIS2_PLACEMENT_3D ( 'NONE', #14550, #21185, #17775 ) ;
#12873 = ORIENTED_EDGE ( 'NONE', *, *, #4449, .F. ) ;
#12874 = CARTESIAN_POINT ( 'NONE',  ( 41.41151635295819489, 107.3156853856626043, 70.85477822274174287 ) ) ;
#12875 = CARTESIAN_POINT ( 'NONE',  ( -89.78587645599536415, 88.03336485954913826, 50.76527035810606492 ) ) ;
#12876 = CARTESIAN_POINT ( 'NONE',  ( -61.89146549900200256, 14.99999999999998579, 89.19471017242423727 ) ) ;
#12877 = CIRCLE ( 'NONE', #3314, 12.37020706055088759 ) ;
#12878 = ADVANCED_FACE ( 'NONE', ( #1730 ), #19176, .T. ) ;
#12879 = VERTEX_POINT ( 'NONE', #6884 ) ;
#12880 = ADVANCED_FACE ( 'NONE', ( #7231 ), #8191, .T. ) ;
#12881 = CARTESIAN_POINT ( 'NONE',  ( 146.4999999999998863, 1.999999999999998224, 8.000000000001989520 ) ) ;
#12882 = VECTOR ( 'NONE', #3265, 1000.000000000000000 ) ;
#12883 = ADVANCED_FACE ( 'NONE', ( #3, #14034, #14259 ), #21132, .F. ) ;
#12884 = DIRECTION ( 'NONE',  ( 5.440186201345738641E-18, 1.000000000000000000, 1.334940939666364181E-17 ) ) ;
#12885 = EDGE_CURVE ( 'NONE', #13489, #11778, #11504, .T. ) ;
#12886 = ORIENTED_EDGE ( 'NONE', *, *, #19241, .T. ) ;
#12887 = CARTESIAN_POINT ( 'NONE',  ( 4.195452682864946325, 166.7895964344300808, 324.5942600080963985 ) ) ;
#12888 = VECTOR ( 'NONE', #11165, 999.9999999999998863 ) ;
#12889 = DIRECTION ( 'NONE',  ( -0.01292394549866739996, -0.005513023399721131770, -0.9999012842304692006 ) ) ;
#12890 = LINE ( 'NONE', #19152, #5459 ) ;
#12891 = EDGE_CURVE ( 'NONE', #21571, #8155, #16553, .T. ) ;
#12892 = DIRECTION ( 'NONE',  ( 7.125109674159588039E-05, -0.9999848031710253382, 0.005512562950848870491 ) ) ;
#12893 = DIRECTION ( 'NONE',  ( -2.025474946048326158E-22, 1.000000000000000000, -1.876735158486679638E-22 ) ) ;
#12894 = ORIENTED_EDGE ( 'NONE', *, *, #19853, .T. ) ;
#12895 = CARTESIAN_POINT ( 'NONE',  ( 19.16751163549090009, 175.4987477760657839, 90.21185077511255201 ) ) ;
#12896 = AXIS2_PLACEMENT_3D ( 'NONE', #21318, #19697, #21532 ) ;
#12897 = EDGE_LOOP ( 'NONE', ( #20388, #4818, #39, #16917 ) ) ;
#12898 = VECTOR ( 'NONE', #5146, 1000.000000000000114 ) ;
#12899 = CARTESIAN_POINT ( 'NONE',  ( 49.29218688498771428, 189.5954397161826535, -74.07991498343932335 ) ) ;
#12900 = CARTESIAN_POINT ( 'NONE',  ( -41.56338128877947469, 170.2445484137435585, 269.1611253287739487 ) ) ;
#12901 = CARTESIAN_POINT ( 'NONE',  ( -10.14484841738276089, 70.07547478993376444, -88.15032624680998197 ) ) ;
#12902 = EDGE_CURVE ( 'NONE', #3576, #3054, #1593, .T. ) ;
#12903 = FACE_OUTER_BOUND ( 'NONE', #2071, .T. ) ;
#12904 = FACE_BOUND ( 'NONE', #15347, .T. ) ;
#12905 = CARTESIAN_POINT ( 'NONE',  ( 45.19547368498248829, 129.3639651298425406, 246.9563529314173707 ) ) ;
#12906 = B_SPLINE_CURVE_WITH_KNOTS ( 'NONE', 3,
 ( #12646, #15990, #1953, #3781, #21228, #7455, #19513, #9396, #119, #7117, #2164, #11137, #9163, #16217, #10804, #338 ),
 .UNSPECIFIED., .F., .F.,
 ( 4, 2, 2, 2, 2, 2, 2, 4 ),
 ( 6.938893903907227607E-18, 0.0004255381963929606411, 0.0008510763927859143433, 0.001276614589178868154, 0.001702152785571821748, 0.002127690981964775775, 0.002553229178357729369, 0.003404305571143620077 ),
 .UNSPECIFIED. ) ;
#12907 = EDGE_CURVE ( 'NONE', #16500, #13344, #21018, .T. ) ;
#12908 = FACE_OUTER_BOUND ( 'NONE', #20421, .T. ) ;
#12909 = ORIENTED_EDGE ( 'NONE', *, *, #21017, .T. ) ;
#12910 = AXIS2_PLACEMENT_3D ( 'NONE', #13578, #2885, #3113 ) ;
#12911 = CARTESIAN_POINT ( 'NONE',  ( 397.1141114976279596, 91.17157287525404286, 77.87414493559184336 ) ) ;
#12912 = EDGE_CURVE ( 'NONE', #9625, #16088, #4871, .T. ) ;
#12913 = CIRCLE ( 'NONE', #15116, 2.000000000000001776 ) ;
#12914 = DIRECTION ( 'NONE',  ( 0.000000000000000000, 0.000000000000000000, 1.000000000000000000 ) ) ;
#12915 = VERTEX_POINT ( 'NONE', #3166 ) ;
#12916 = AXIS2_PLACEMENT_3D ( 'NONE', #4280, #14782, #2576 ) ;
#12917 = EDGE_LOOP ( 'NONE', ( #5143, #12036, #1160, #14907 ) ) ;
#12918 = CARTESIAN_POINT ( 'NONE',  ( -81.38707033994185736, 75.12824275668154428, -3.883447788322965444 ) ) ;
#12919 = CARTESIAN_POINT ( 'NONE',  ( -88.16289161317095591, 88.20043279625843979, 52.96119657702186601 ) ) ;
#12920 = VECTOR ( 'NONE', #12968, 1000.000000000000227 ) ;
#12922 = EDGE_LOOP ( 'NONE', ( #3418, #10924, #16124, #17493, #2433 ) ) ;
#12921 = VERTEX_POINT ( 'NONE', #15164 ) ;
#12923 = ORIENTED_EDGE ( 'NONE', *, *, #10434, .F. ) ;
#12924 = EDGE_CURVE ( 'NONE', #10057, #17159, #11583, .T. ) ;
#12925 = CARTESIAN_POINT ( 'NONE',  ( -45.96219963993937796, 168.0879242961143518, -74.15276576609245751 ) ) ;
#12926 = CIRCLE ( 'NONE', #7409, 2.000000000000001332 ) ;
#12927 = DIRECTION ( 'NONE',  ( 7.125109674364534776E-05, -0.9999848031710252272, 0.005512562950849704893 ) ) ;
#12928 = AXIS2_PLACEMENT_3D ( 'NONE', #22558, #13657, #8573 ) ;
#12929 = CARTESIAN_POINT ( 'NONE',  ( 68.43148148480361215, 69.99999999999998579, 86.12277481476651531 ) ) ;
#12930 = DIRECTION ( 'NONE',  ( 0.9999164797902015955, 6.965998958219364448E-18, -0.01292414190464157182 ) ) ;
#12931 = CARTESIAN_POINT ( 'NONE',  ( 73.74384038452764401, 74.99999999999998579, -0.9531554654672949045 ) ) ;
#12932 = TOROIDAL_SURFACE ( 'NONE', #4094, 10.00000000000000178, 2.272904689641331188 ) ;
#12933 = CARTESIAN_POINT ( 'NONE',  ( 18.80756281266039665, 183.8219316425800685, 318.0440155801259721 ) ) ;
#12934 = CARTESIAN_POINT ( 'NONE',  ( 20.17774460750976928, 88.61083286335994558, -77.93556127472962203 ) ) ;
#12935 = CARTESIAN_POINT ( 'NONE',  ( -38.79722561300751238, 125.3640259171584290, 248.0640311032106524 ) ) ;
#12936 = ORIENTED_EDGE ( 'NONE', *, *, #11653, .F. ) ;
#12937 =( LENGTH_UNIT ( ) NAMED_UNIT ( * ) SI_UNIT ( .MILLI., .METRE. ) );
#12938 = AXIS2_PLACEMENT_3D ( 'NONE', #3570, #6570, #18962 ) ;
#12939 = APPLICATION_CONTEXT ( 'automotive_design' ) ;
#12940 = EDGE_CURVE ( 'NONE', #15089, #7368, #4133, .T. ) ;
#12941 = CYLINDRICAL_SURFACE ( 'NONE', #6280, 78.99999999999998579 ) ;
#12942 = CARTESIAN_POINT ( 'NONE',  ( -10.01265065029762980, 187.8784833776788332, 308.1592754748398875 ) ) ;
#12943 = ORIENTED_EDGE ( 'NONE', *, *, #6764, .T. ) ;
#12944 = CARTESIAN_POINT ( 'NONE',  ( 93.23587179807657321, 72.00000000000000000, 30.79757858250317781 ) ) ;
#12945 = VERTEX_POINT ( 'NONE', #1577 ) ;
#12946 = EDGE_LOOP ( 'NONE', ( #2254, #14153, #15155, #14464 ) ) ;
#12947 = CIRCLE ( 'NONE', #6688, 2.000000000000001332 ) ;
#12948 = DIRECTION ( 'NONE',  ( 0.9934404589540163366, 0.1135548637187053511, -0.01346653032743023309 ) ) ;
#12949 = CARTESIAN_POINT ( 'NONE',  ( -29.71368853164436530, 55.00725983767640770, -132.4039035450188351 ) ) ;
#12950 = ORIENTED_EDGE ( 'NONE', *, *, #19618, .F. ) ;
#12951 = AXIS2_PLACEMENT_3D ( 'NONE', #1165, #15190, #6542 ) ;
#12952 = LINE ( 'NONE', #18319, #15096 ) ;
#12953 = CARTESIAN_POINT ( 'NONE',  ( 75.13896584913651111, 75.01394013563931651, -2.606578332019783506 ) ) ;
#12954 = CARTESIAN_POINT ( 'NONE',  ( -90.01145195396890131, 71.38761518557662100, 62.48983541110989393 ) ) ;
#12955 = CARTESIAN_POINT ( 'NONE',  ( 76.24440817582265595, 75.12974839299529606, 3.983549157388267759 ) ) ;
#12956 = DIRECTION ( 'NONE',  ( 0.7912924530843116200, -0.6113994113550571541, -0.006856638134102505111 ) ) ;
#12957 = ORIENTED_EDGE ( 'NONE', *, *, #20558, .F. ) ;
#12958 = CARTESIAN_POINT ( 'NONE',  ( -68.71681667565952978, 91.32006346413032816, 85.89527988174788220 ) ) ;
#12959 = DIRECTION ( 'NONE',  ( 0.000000000000000000, 0.000000000000000000, 1.000000000000000000 ) ) ;
#12960 = AXIS2_PLACEMENT_3D ( 'NONE', #1821, #18034, #16210 ) ;
#12961 = DIRECTION ( 'NONE',  ( 0.1136178953597573593, -0.9935164314186355483, 0.004009283626633517415 ) ) ;
#12962 = AXIS2_PLACEMENT_3D ( 'NONE', #6218, #19653, #10940 ) ;
#12963 = DIRECTION ( 'NONE',  ( -0.8981428216242030027, 0.000000000000000000, -0.4397038457472430273 ) ) ;
#12964 = DIRECTION ( 'NONE',  ( -0.000000000000000000, -1.000000000000000000, -0.000000000000000000 ) ) ;
#12965 = CARTESIAN_POINT ( 'NONE',  ( -91.18811779502803461, 77.39015272472282447, 31.60719401330432277 ) ) ;
#12966 = CARTESIAN_POINT ( 'NONE',  ( 44.03028354117878251, 168.0879242961143518, -75.31593853751020617 ) ) ;
#12967 = VERTEX_POINT ( 'NONE', #10187 ) ;
#12968 = DIRECTION ( 'NONE',  ( -0.7912924530843117310, 0.6113994113550571541, 0.006856638134102506846 ) ) ;
#12969 = EDGE_CURVE ( 'NONE', #3481, #7202, #16868, .T. ) ;
#12970 = LINE ( 'NONE', #2612, #5136 ) ;
#12971 = VECTOR ( 'NONE', #10794, 1000.000000000000114 ) ;
#12972 = B_SPLINE_CURVE_WITH_KNOTS ( 'NONE', 3,
 ( #18073, #19425, #603, #16021, #12776, #7487 ),
 .UNSPECIFIED., .F., .F.,
 ( 4, 2, 4 ),
 ( 0.008070723795061282568, 0.009531773844229259746, 0.01099282389339723866 ),
 .UNSPECIFIED. ) ;
#12973 = CARTESIAN_POINT ( 'NONE',  ( -9.373580856408977979, 184.8150131700745646, 307.9996070035269327 ) ) ;
#12974 = ADVANCED_FACE ( 'NONE', ( #17315 ), #22550, .T. ) ;
#12975 = ORIENTED_EDGE ( 'NONE', *, *, #5547, .T. ) ;
#12976 = EDGE_LOOP ( 'NONE', ( #1831, #22487, #15394, #2153 ) ) ;
#12977 = CARTESIAN_POINT ( 'NONE',  ( -93.23587179807654479, 72.00000000000000000, -30.79757858250321689 ) ) ;
#12978 = CIRCLE ( 'NONE', #3048, 117.0000000000000000 ) ;
#12979 = AXIS2_PLACEMENT_3D ( 'NONE', #13246, #1510, #6555 ) ;
#12980 = FACE_OUTER_BOUND ( 'NONE', #5218, .T. ) ;
#12981 = CONTEXT_DEPENDENT_SHAPE_REPRESENTATION ( #8371, #17277 ) ;
#12982 = CARTESIAN_POINT ( 'NONE',  ( 55.40268456415107323, 1.999999999999998224, -113.1659955246503557 ) ) ;
#12983 = DIRECTION ( 'NONE',  ( -7.125109674159588039E-05, 0.9999848031710253382, -0.005512562950848870491 ) ) ;
#12984 = EDGE_LOOP ( 'NONE', ( #3217, #15969, #6183, #10158 ) ) ;
#12985 = VECTOR ( 'NONE', #20085, 1000.000000000000227 ) ;
#12986 = VECTOR ( 'NONE', #22092, 999.9999999999998863 ) ;
#12987 = ORIENTED_EDGE ( 'NONE', *, *, #14860, .F. ) ;
#12988 = CARTESIAN_POINT ( 'NONE',  ( -41.07974036897499559, 106.8060942374655156, 71.47017004102838200 ) ) ;
#12989 = ORIENTED_EDGE ( 'NONE', *, *, #11680, .T. ) ;
#12990 = CARTESIAN_POINT ( 'NONE',  ( -15.56353044989331735, 177.7370943402667649, 314.3607490585801543 ) ) ;
#12991 = ORIENTED_EDGE ( 'NONE', *, *, #22117, .T. ) ;
#12992 = DIRECTION ( 'NONE',  ( 0.000000000000000000, 0.000000000000000000, 1.000000000000000000 ) ) ;
#12993 = CARTESIAN_POINT ( 'NONE',  ( -40.73077958905026463, 95.66828137409537192, -42.40511349254944662 ) ) ;
#12994 = CARTESIAN_POINT ( 'NONE',  ( -19.28847592064633787, 309.3375565838056787, 328.6122914246403184 ) ) ;
#12995 = VECTOR ( 'NONE', #625, 1000.000000000000114 ) ;
#12996 = EDGE_LOOP ( 'NONE', ( #11684, #13661, #11937, #15230 ) ) ;
#12997 = AXIS2_PLACEMENT_3D ( 'NONE', #16744, #2596, #16510 ) ;
#12998 = DIRECTION ( 'NONE',  ( 0.000000000000000000, 0.000000000000000000, 1.000000000000000000 ) ) ;
#12999 = EDGE_CURVE ( 'NONE', #10113, #4456, #18681, .T. ) ;
#13000 = CARTESIAN_POINT ( 'NONE',  ( -1.446236478174511397, 81.98100004360546222, -80.95361029988728774 ) ) ;
#13001 = VERTEX_POINT ( 'NONE', #8564 ) ;
#13002 = CIRCLE ( 'NONE', #15943, 120.0000000000000000 ) ;
#13003 = AXIS2_PLACEMENT_3D ( 'NONE', #3098, #1041, #1499 ) ;
#13004 = UNCERTAINTY_MEASURE_WITH_UNIT (LENGTH_MEASURE( 1.000000000000000082E-05 ), #17328, 'distance_accuracy_value', 'NONE');
#13005 = CARTESIAN_POINT ( 'NONE',  ( 40.97829051141438583, 107.9174786211642214, 71.38475741957512355 ) ) ;
#13006 = CARTESIAN_POINT ( 'NONE',  ( -89.82557373136849321, 87.98571510324423173, 50.79485365709339106 ) ) ;
#13007 = APPLICATION_PROTOCOL_DEFINITION ( 'draft international standard', 'automotive_design', 1998, #3389 ) ;
#13008 = VECTOR ( 'NONE', #20856, 1000.000000000000000 ) ;
#13010 = EDGE_LOOP ( 'NONE', ( #14791, #14982, #3101, #16031 ) ) ;
#13009 = ORIENTED_EDGE ( 'NONE', *, *, #12902, .F. ) ;
#13011 = AXIS2_PLACEMENT_3D ( 'NONE', #6755, #19150, #8808 ) ;
#13012 = CARTESIAN_POINT ( 'NONE',  ( 51.78636885665599010, 152.2590373701828241, 256.0525387646090394 ) ) ;
#13013 = EDGE_CURVE ( 'NONE', #22296, #7530, #14445, .T. ) ;
#13014 = CARTESIAN_POINT ( 'NONE',  ( -52.71146364212827962, 109.8959631047793124, -43.49169827137859556 ) ) ;
#13015 = B_SPLINE_CURVE_WITH_KNOTS ( 'NONE', 3,
 ( #22637, #12246, #12011, #20614 ),
 .UNSPECIFIED., .F., .F.,
 ( 4, 4 ),
 ( 0.000000000000000000, 0.001461243987308227452 ),
 .UNSPECIFIED. ) ;
#13016 = VERTEX_POINT ( 'NONE', #8130 ) ;
#13017 = DIRECTION ( 'NONE',  ( 0.9934404589540163366, 0.1135548637187057258, -0.01346653032743021922 ) ) ;
#13018 = CARTESIAN_POINT ( 'NONE',  ( 11.48281922048859727, 176.2279375523750957, 299.4455621116320003 ) ) ;
#13019 = CARTESIAN_POINT ( 'NONE',  ( -106.1519489938925602, 71.09828217887417168, -28.84036442345827922 ) ) ;
#13020 = CARTESIAN_POINT ( 'NONE',  ( 86.79222083800954124, 104.3814432989690602, 67.58039954014910222 ) ) ;
#13021 = DIRECTION ( 'NONE',  ( -7.125109674118361251E-05, 0.9999848031710253382, -0.005512562950849477644 ) ) ;
#13022 = VERTEX_POINT ( 'NONE', #3274 ) ;
#13023 = CARTESIAN_POINT ( 'NONE',  ( 34.61804907780420848, 94.93197183469659706, -82.52232902628021805 ) ) ;
#13024 = EDGE_LOOP ( 'NONE', ( #18296, #13871 ) ) ;
#13025 = CARTESIAN_POINT ( 'NONE',  ( -68.71681667565952978, 69.99999999999998579, 85.89527988174785378 ) ) ;
#13026 = FACE_BOUND ( 'NONE', #13868, .T. ) ;
#13027 = TOROIDAL_SURFACE ( 'NONE', #7868, -102.0000000000000000, 120.0000000000000000 ) ;
#13028 = CARTESIAN_POINT ( 'NONE',  ( -90.00000000000000000, 45.00100000000000477, 8.394090934816448357E-16 ) ) ;
#13029 = CARTESIAN_POINT ( 'NONE',  ( 79.99331838321626265, 100.9999999999999858, -7.033931352371318724 ) ) ;
#13030 = FACE_OUTER_BOUND ( 'NONE', #6908, .T. ) ;
#13031 = ORIENTED_EDGE ( 'NONE', *, *, #7815, .F. ) ;
#13032 = FACE_OUTER_BOUND ( 'NONE', #10148, .T. ) ;
#13033 = CARTESIAN_POINT ( 'NONE',  ( 50.77011715189885166, 106.9149828242082947, 59.25939429586269824 ) ) ;
#13034 = CIRCLE ( 'NONE', #20703, 102.6746853779045381 ) ;
#13035 = DIRECTION ( 'NONE',  ( 0.000000000000000000, 0.000000000000000000, 1.000000000000000000 ) ) ;
#13036 = EDGE_CURVE ( 'NONE', #18327, #11619, #22095, .T. ) ;
#13037 = ORIENTED_EDGE ( 'NONE', *, *, #3904, .T. ) ;
#13038 = AXIS2_PLACEMENT_3D ( 'NONE', #15623, #20991, #14361 ) ;
#13039 = PLANE ( 'NONE',  #5784 ) ;
#13040 = ADVANCED_FACE ( 'NONE', ( #13428 ), #11689, .F. ) ;
#13041 = ORIENTED_EDGE ( 'NONE', *, *, #8919, .T. ) ;
#13042 = ORIENTED_EDGE ( 'NONE', *, *, #18627, .T. ) ;
#13043 = DIRECTION ( 'NONE',  ( -0.9232306267972776315, 0.000000000000000000, 0.3842462878721224495 ) ) ;
#13044 = CARTESIAN_POINT ( 'NONE',  ( -90.14332777612271741, 88.20948563679688448, 52.98067045136929920 ) ) ;
#13045 = MECHANICAL_DESIGN_GEOMETRIC_PRESENTATION_REPRESENTATION (  '', ( #18876 ), #22173 ) ;
#13046 = VERTEX_POINT ( 'NONE', #3068 ) ;
#13047 = ADVANCED_FACE ( 'NONE', ( #17098 ), #20634, .F. ) ;
#13048 = DIRECTION ( 'NONE',  ( 0.9915597537056654032, -0.0006440578489082665614, -0.1296489106033952843 ) ) ;
#13049 = DIRECTION ( 'NONE',  ( -0.01292394549866695240, -0.005513023399718316314, -0.9999012842304693116 ) ) ;
#13050 = DIRECTION ( 'NONE',  ( -0.009138748381789112835, -0.7071067811865462405, -0.7070477234798343558 ) ) ;
#13051 = EDGE_CURVE ( 'NONE', #2469, #10602, #4499, .T. ) ;
#13052 = ORIENTED_EDGE ( 'NONE', *, *, #2384, .F. ) ;
#13053 = LINE ( 'NONE', #21835, #5495 ) ;
#13054 = FACE_OUTER_BOUND ( 'NONE', #1625, .T. ) ;
#13055 = CARTESIAN_POINT ( 'NONE',  ( 19.41230309865470716, 184.3421512348843692, 316.6627316332904343 ) ) ;
#13056 = CARTESIAN_POINT ( 'NONE',  ( 28.61719497298777526, 91.18493411151780492, -80.66446637815775489 ) ) ;
#13057 = DIRECTION ( 'NONE',  ( -0.7161863329816273716, -0.003898296230782334528, -0.6978982302147116457 ) ) ;
#13058 = ORIENTED_EDGE ( 'NONE', *, *, #1695, .T. ) ;
#13059 = CARTESIAN_POINT ( 'NONE',  ( 91.45377919752198181, 96.73472523269998646, 61.12462174243592727 ) ) ;
#13060 = EDGE_CURVE ( 'NONE', #9463, #4144, #14219, .T. ) ;
#13061 = EDGE_CURVE ( 'NONE', #2491, #15391, #3051, .T. ) ;
#13062 = CARTESIAN_POINT ( 'NONE',  ( 63.92222308695262711, 94.02752048664900997, -83.80561885825635215 ) ) ;
#13063 = DIRECTION ( 'NONE',  ( -5.440186201345738641E-18, -1.000000000000000000, -1.334940939666364181E-17 ) ) ;
#13064 = ORIENTED_EDGE ( 'NONE', *, *, #4686, .T. ) ;
#13065 = CARTESIAN_POINT ( 'NONE',  ( -1.163172771417702700, 81.99999999999998579, -89.99248318111824574 ) ) ;
#13066 = EDGE_LOOP ( 'NONE', ( #18090, #20063, #20889 ) ) ;
#13067 = VERTEX_POINT ( 'NONE', #19250 ) ;
#13068 = CARTESIAN_POINT ( 'NONE',  ( 12.46561401535050528, 167.6340204206038891, 299.4802424150023512 ) ) ;
#13069 = LINE ( 'NONE', #14912, #9942 ) ;
#13070 = DIRECTION ( 'NONE',  ( 0.9999164797902015955, 6.965998958219364448E-18, -0.01292414190464157182 ) ) ;
#13071 = AXIS2_PLACEMENT_3D ( 'NONE', #16559, #6429, #8145 ) ;
#13072 = ADVANCED_FACE ( 'NONE', ( #17895 ), #1693, .F. ) ;
#13073 = CARTESIAN_POINT ( 'NONE',  ( 73.74911173825391586, 74.99999999999995737, -0.5453207712484345882 ) ) ;
#13074 = FACE_BOUND ( 'NONE', #13941, .T. ) ;
#13075 = EDGE_CURVE ( 'NONE', #12626, #10931, #5529, .T. ) ;
#13076 = EDGE_LOOP ( 'NONE', ( #2004, #15538, #19019, #12269, #21198, #13698 ) ) ;
#13077 = DIRECTION ( 'NONE',  ( -0.01292394549866739996, -0.005513023399721131770, -0.9999012842304692006 ) ) ;
#13078 = DIRECTION ( 'NONE',  ( 0.000000000000000000, 0.000000000000000000, 1.000000000000000000 ) ) ;
#13079 = LINE ( 'NONE', #335, #18119 ) ;
#13080 = DIRECTION ( 'NONE',  ( 0.9999164797902015955, 6.965998958219364448E-18, -0.01292414190464157182 ) ) ;
#13081 = CARTESIAN_POINT ( 'NONE',  ( 92.02635692360502162, 79.83422912033846330, -31.21470397902952598 ) ) ;
#13082 = CARTESIAN_POINT ( 'NONE',  ( 79.99331838321640475, 84.99999999999997158, -1.033931352371301848 ) ) ;
#13083 = ORIENTED_EDGE ( 'NONE', *, *, #5387, .F. ) ;
#13084 = DIRECTION ( 'NONE',  ( 0.9232306267972774094, 0.000000000000000000, -0.3842462878721227826 ) ) ;
#13085 = EDGE_CURVE ( 'NONE', #12094, #858, #17758, .T. ) ;
#13086 = DIRECTION ( 'NONE',  ( 7.125109674160258889E-05, -0.9999848031710253382, 0.005512562950849898315 ) ) ;
#13087 = CARTESIAN_POINT ( 'NONE',  ( -14.08815279242220520, 180.1090064943867333, 310.9205019102012670 ) ) ;
#13088 = ORIENTED_EDGE ( 'NONE', *, *, #7659, .T. ) ;
#13089 = VECTOR ( 'NONE', #8368, 1000.000000000000000 ) ;
#13090 = VERTEX_POINT ( 'NONE', #10527 ) ;
#13091 = FACE_BOUND ( 'NONE', #13452, .T. ) ;
#13092 = CARTESIAN_POINT ( 'NONE',  ( 2.775557561562891351E-13, 84.99999999999997158, 4.271756559592887470E-14 ) ) ;
#13093 = CARTESIAN_POINT ( 'NONE',  ( 146.5000000000000000, 20.00000000000000000, -2.025191382850354537E-12 ) ) ;
#13094 = EDGE_CURVE ( 'NONE', #17125, #163, #10390, .T. ) ;
#13095 = ADVANCED_FACE ( 'NONE', ( #6951 ), #8905, .F. ) ;
#13096 = CARTESIAN_POINT ( 'NONE',  ( -46.77031037318527495, 119.7725967263615985, 250.1981111634296155 ) ) ;
#13097 = ORIENTED_EDGE ( 'NONE', *, *, #5993, .F. ) ;
#13098 = ORIENTED_EDGE ( 'NONE', *, *, #1377, .F. ) ;
#13099 = CARTESIAN_POINT ( 'NONE',  ( 82.50899511402293740, 104.9527666485724922, -72.74866258673912967 ) ) ;
#13100 = VERTEX_POINT ( 'NONE', #12264 ) ;
#13101 = CARTESIAN_POINT ( 'NONE',  ( -9.608651860293715430, 184.6439102242405284, 305.3492338956228309 ) ) ;
#13102 = FACE_OUTER_BOUND ( 'NONE', #16512, .T. ) ;
#13103 = CARTESIAN_POINT ( 'NONE',  ( 12.18267571817558981, 187.8048479060753948, 322.6837437219421076 ) ) ;
#13104 = CARTESIAN_POINT ( 'NONE',  ( -40.60272855283507454, 95.87258248339890088, -42.05554350543408759 ) ) ;
#13105 = CARTESIAN_POINT ( 'NONE',  ( -157.5176307659779411, 20.00000000000000000, -60.94675664190619813 ) ) ;
#13106 = DIRECTION ( 'NONE',  ( -0.01292394549866632963, -0.005513023399716958026, -0.9999012842304692006 ) ) ;
#13107 = ORIENTED_EDGE ( 'NONE', *, *, #881, .F. ) ;
#13108 = CARTESIAN_POINT ( 'NONE',  ( -1.109343863968193944E-13, 18.00000000000000355, -7.999999999999994671 ) ) ;
#13109 = CARTESIAN_POINT ( 'NONE',  ( -88.17103187914774765, 88.81848268355626885, 52.20485361863669027 ) ) ;
#13110 = APPLICATION_PROTOCOL_DEFINITION ( 'draft international standard', 'automotive_design', 1998, #15292 ) ;
#13111 = EDGE_LOOP ( 'NONE', ( #13502, #4018 ) ) ;
#13112 = CARTESIAN_POINT ( 'NONE',  ( 48.76804916713667382, 169.4762627770265340, -95.63682909712669300 ) ) ;
#13113 = EDGE_CURVE ( 'NONE', #14836, #13307, #8904, .T. ) ;
#13114 = CARTESIAN_POINT ( 'NONE',  ( 90.41042953090175160, 78.34730160488619788, -33.05240787946388537 ) ) ;
#13115 = LINE ( 'NONE', #18504, #12985 ) ;
#13116 = CYLINDRICAL_SURFACE ( 'NONE', #19508, 22.50000000000000000 ) ;
#13117 = CARTESIAN_POINT ( 'NONE',  ( 51.99565694909048830, 170.0000000000000284, -0.6720553790413839046 ) ) ;
#13118 = LINE ( 'NONE', #13560, #590 ) ;
#13119 = DIRECTION ( 'NONE',  ( 0.9909299940865186063, -0.1338359446631180727, -0.01207007604876311237 ) ) ;
#13120 = CARTESIAN_POINT ( 'NONE',  ( 69.33518156588188219, 92.50622784628018280, -85.39700225480594042 ) ) ;
#13121 = ORIENTED_EDGE ( 'NONE', *, *, #20858, .T. ) ;
#13122 = CARTESIAN_POINT ( 'NONE',  ( -65.35548625431930247, 98.86074611927202227, 78.99051476369086799 ) ) ;
#13123 = ORIENTED_EDGE ( 'NONE', *, *, #349, .F. ) ;
#13124 = CARTESIAN_POINT ( 'NONE',  ( 14.08568026761702896, 137.6763543404365180, 122.6003119075071197 ) ) ;
#13125 = DIRECTION ( 'NONE',  ( 0.9999164797902017066, 2.001050586450178931E-22, -0.01292414190464131508 ) ) ;
#13126 = DIRECTION ( 'NONE',  ( 0.1296504907605110779, 0.005475273188902231650, 0.9915446392518419971 ) ) ;
#13127 = FACE_OUTER_BOUND ( 'NONE', #19192, .T. ) ;
#13128 = VECTOR ( 'NONE', #1536, 1000.000000000000114 ) ;
#13129 = ORIENTED_EDGE ( 'NONE', *, *, #9657, .T. ) ;
#13130 = FACE_OUTER_BOUND ( 'NONE', #10663, .T. ) ;
#13131 = DIRECTION ( 'NONE',  ( -0.5439613279325644646, -0.8390293148633950482, 0.01165686551792462916 ) ) ;
#13132 = CARTESIAN_POINT ( 'NONE',  ( -51.88145199138811137, 111.6854492628015976, -46.70071095239993042 ) ) ;
#13133 = ORIENTED_EDGE ( 'NONE', *, *, #20639, .T. ) ;
#13134 = CARTESIAN_POINT ( 'NONE',  ( 12.84376896873858875, 190.4863203672247494, 307.8501947603993472 ) ) ;
#13135 = ORIENTED_EDGE ( 'NONE', *, *, #11600, .F. ) ;
#13136 = ORIENTED_EDGE ( 'NONE', *, *, #19314, .T. ) ;
#13137 = CARTESIAN_POINT ( 'NONE',  ( -84.79288518521889273, 75.01682528584525755, -0.6987393684433246266 ) ) ;
#13138 = CARTESIAN_POINT ( 'NONE',  ( -88.16204873317377633, 88.10266582584259254, 53.02941603701640361 ) ) ;
#13139 = ORIENTED_EDGE ( 'NONE', *, *, #21603, .F. ) ;
#13140 = EDGE_CURVE ( 'NONE', #11555, #1979, #7826, .T. ) ;
#13141 = AXIS2_PLACEMENT_3D ( 'NONE', #1619, #15877, #1957 ) ;
#13142 = CARTESIAN_POINT ( 'NONE',  ( -37.35473898174801377, 105.5788163333585743, 92.63175017747209949 ) ) ;
#13143 = AXIS2_PLACEMENT_3D ( 'NONE', #196, #16302, #19251 ) ;
#13144 = CARTESIAN_POINT ( 'NONE',  ( 153.9999999999992610, 20.00000000000000000, 53.76161406891468175 ) ) ;
#13145 = PLANE ( 'NONE',  #1789 ) ;
#13146 = ADVANCED_FACE ( 'NONE', ( #10870 ), #20848, .T. ) ;
#13147 = FACE_OUTER_BOUND ( 'NONE', #8618, .T. ) ;
#13148 = FACE_OUTER_BOUND ( 'NONE', #19757, .T. ) ;
#13149 = ADVANCED_FACE ( 'NONE', ( #12141, #3622, #19127, #20966 ), #8779, .F. ) ;
#13150 = ORIENTED_EDGE ( 'NONE', *, *, #17235, .T. ) ;
#13151 = EDGE_CURVE ( 'NONE', #18898, #1217, #9296, .T. ) ;
#13152 = DIRECTION ( 'NONE',  ( -0.01292394549866740863, -0.005513023399721009472, -0.9999012842304692006 ) ) ;
#13153 = DIRECTION ( 'NONE',  ( -0.01292394549866750231, -0.005513023399722823126, -0.9999012842304692006 ) ) ;
#13154 = CARTESIAN_POINT ( 'NONE',  ( 17.97637993448925542, 184.5224678489072119, 318.9840103354205780 ) ) ;
#13155 = LINE ( 'NONE', #18432, #8127 ) ;
#13156 = AXIS2_PLACEMENT_3D ( 'NONE', #14759, #497, #21711 ) ;
#13157 = FACE_OUTER_BOUND ( 'NONE', #3488, .T. ) ;
#13158 = CARTESIAN_POINT ( 'NONE',  ( 48.64240681911486774, 159.4614951111008452, 276.0554384422054000 ) ) ;
#13159 = ORIENTED_EDGE ( 'NONE', *, *, #14588, .F. ) ;
#13160 = ADVANCED_FACE ( 'NONE', ( #14105 ), #21087, .F. ) ;
#13161 = DIRECTION ( 'NONE',  ( 0.009760756503427813965, -0.9999378516499565217, 0.005387065077607405654 ) ) ;
#13162 = DIRECTION ( 'NONE',  ( 0.01292394549866738782, 0.005513023399720700692, 0.9999012842304693116 ) ) ;
#13163 = ORIENTED_EDGE ( 'NONE', *, *, #7445, .T. ) ;
#13164 = DIRECTION ( 'NONE',  ( -0.9909299940865189393, 0.1338359446631160188, 0.01207007604876292328 ) ) ;
#13165 = VERTEX_POINT ( 'NONE', #3744 ) ;
#13166 = DIRECTION ( 'NONE',  ( 0.01292394549866705648, 0.005513023399720703294, 0.9999012842304692006 ) ) ;
#13167 = EDGE_CURVE ( 'NONE', #5531, #1407, #20835, .T. ) ;
#13168 = ORIENTED_EDGE ( 'NONE', *, *, #7950, .T. ) ;
#13169 = VECTOR ( 'NONE', #4382, 1000.000000000000114 ) ;
#13170 = VERTEX_POINT ( 'NONE', #10760 ) ;
#13171 = AXIS2_PLACEMENT_3D ( 'NONE', #177, #7171, #394 ) ;
#13172 = DIRECTION ( 'NONE',  ( -0.01292394549866728373, -0.005513023399720296501, -0.9999012842304693116 ) ) ;
#13173 = DIRECTION ( 'NONE',  ( -1.000000000000000000, 0.000000000000000000, 1.386679829960243376E-14 ) ) ;
#13174 = DIRECTION ( 'NONE',  ( -0.000000000000000000, -1.000000000000000000, -0.000000000000000000 ) ) ;
#13175 = EDGE_CURVE ( 'NONE', #18739, #17190, #14481, .T. ) ;
#13176 = CARTESIAN_POINT ( 'NONE',  ( 74.09836678676883537, 75.02106928012277365, 1.052672645090043879 ) ) ;
#13177 = PLANE ( 'NONE',  #2335 ) ;
#13178 = EDGE_CURVE ( 'NONE', #21686, #6519, #4516, .T. ) ;
#13179 = VERTEX_POINT ( 'NONE', #7540 ) ;
#13180 = EDGE_CURVE ( 'NONE', #7438, #10504, #21403, .T. ) ;
#13181 = CARTESIAN_POINT ( 'NONE',  ( 111.9405537842442300, 11.64346788815265299, -314.6407045341634330 ) ) ;
#13182 = DIRECTION ( 'NONE',  ( 0.01292394549866739996, 0.005513023399721131770, 0.9999012842304692006 ) ) ;
#13183 = CARTESIAN_POINT ( 'NONE',  ( -40.07963149416921311, 107.0053247559780090, 71.63428818222637062 ) ) ;
#13184 = EDGE_CURVE ( 'NONE', #14396, #20688, #2478, .T. ) ;
#13185 = CARTESIAN_POINT ( 'NONE',  ( 91.18811779502807724, 77.39015272472096285, -31.60719401330434764 ) ) ;
#13186 = CARTESIAN_POINT ( 'NONE',  ( -8.348562176644710675, 185.3620174482674088, 323.2531432398233164 ) ) ;
#13187 = DIRECTION ( 'NONE',  ( 0.000000000000000000, 0.000000000000000000, 1.000000000000000000 ) ) ;
#13188 = ORIENTED_EDGE ( 'NONE', *, *, #16705, .T. ) ;
#13189 = VECTOR ( 'NONE', #14539, 1000.000000000000000 ) ;
#13190 = LINE ( 'NONE', #9621, #12920 ) ;
#13191 = EDGE_LOOP ( 'NONE', ( #2122, #14050 ) ) ;
#13192 = DIRECTION ( 'NONE',  ( -9.912705577010318154E-17, 0.000000000000000000, -1.000000000000000000 ) ) ;
#13193 = CARTESIAN_POINT ( 'NONE',  ( -8.921762758010784111, 185.1413007774065989, 305.2050614739068237 ) ) ;
#13194 = ORIENTED_EDGE ( 'NONE', *, *, #13735, .F. ) ;
#13195 = ORIENTED_EDGE ( 'NONE', *, *, #21158, .T. ) ;
#13196 = EDGE_CURVE ( 'NONE', #19195, #4059, #887, .T. ) ;
#13197 = CARTESIAN_POINT ( 'NONE',  ( -67.26198047107922662, 70.17996908938924605, 87.03937574298602442 ) ) ;
#13198 = CLOSED_SHELL ( 'NONE', ( #14461, #8574, #6053, #16940, #19437, #3993, #6002, #5252, #2755, #16718, #15688, #15205, #4192, #13861, #19914, #8866, #289, #10184, #16949, #6428, #5970, #8810, #3375, #22571, #20413, #19059, #13356, #15300, #9267, #4322, #5743, #22045, #12766, #11775, #2075, #1515, #18222, #19342, #16003, #9814, #7600, #12325, #10916, #21270, #17554, #14446, #13995, #2450, #13095, #22651, #7235, #13549, #6397, #6681, #22528, #16250, #2816, #8229, #22418, #5597, #5390, #18357, #8962, #22119, #14007, #3606, #9498, #7135, #17211, #12600, #6035, #9173, #9087, #4695, #8771, #16871, #11097, #8524, #6821, #8030, #4708, #647, #5988, #1156, #5333, #10505, #4060, #1444, #4312, #21012, #11596, #11737, #7399, #15144, #17833, #14063, #13905, #12306, #14797, #17503, #18101, #2639, #14529, #17747, #3976, #8613, #20340, #18344, #319, #6114, #13409, #15606, #15062, #21960, #20843, #2738, #18511, #12442, #11307, #14656, #21517, #19308, #17713, #9639 ) ) ;
#13199 = AXIS2_PLACEMENT_3D ( 'NONE', #3625, #14109, #12491 ) ;
#13200 = LINE ( 'NONE', #18152, #16285 ) ;
#13201 = ADVANCED_FACE ( 'NONE', ( #2377 ), #21748, .T. ) ;
#13202 = TOROIDAL_SURFACE ( 'NONE', #7307, 12.37020706055088759, 2.000000000000000000 ) ;
#13203 = DIRECTION ( 'NONE',  ( -2.025474946048326158E-22, 1.000000000000000000, -1.876735158486679638E-22 ) ) ;
#13204 = B_SPLINE_CURVE_WITH_KNOTS ( 'NONE', 3,
 ( #13485, #4834, #11873, #3125, #10144, #17147, #16396, #14908, #21958, #8091, #14794, #21850, #6257, #13283, #21741, #2470 ),
 .UNSPECIFIED., .F., .F.,
 ( 4, 2, 2, 2, 2, 2, 2, 4 ),
 ( 0.000000000000000000, 0.0009078963835536053763, 0.001815792767107210753, 0.002723689150660815912, 0.003631585534214421505, 0.004539481917768027099, 0.005447378301321631824, 0.007263171068428882909 ),
 .UNSPECIFIED. ) ;
#13205 = ORIENTED_EDGE ( 'NONE', *, *, #16128, .T. ) ;
#13206 = DIRECTION ( 'NONE',  ( -0.01292394549866739996, -0.005513023399721131770, -0.9999012842304692006 ) ) ;
#13207 = CARTESIAN_POINT ( 'NONE',  ( -15.41639432518098829, 177.9592009253594256, 316.4977043549463929 ) ) ;
#13208 = ORIENTED_EDGE ( 'NONE', *, *, #510, .T. ) ;
#13209 = ORIENTED_EDGE ( 'NONE', *, *, #13722, .T. ) ;
#13210 = CARTESIAN_POINT ( 'NONE',  ( -106.4939345422101979, 78.92840590577348792, -27.55192737125463509 ) ) ;
#13211 = CARTESIAN_POINT ( 'NONE',  ( -38.64934902010026008, 96.64904989519661171, 84.47978658464403168 ) ) ;
#13212 = CARTESIAN_POINT ( 'NONE',  ( -109.0842784177615101, 103.0000000000000000, 71.55850894251706507 ) ) ;
#13213 = VERTEX_POINT ( 'NONE', #19802 ) ;
#13214 = CARTESIAN_POINT ( 'NONE',  ( 90.02055463237803679, 34.61572286322119396, -63.21629334023821656 ) ) ;
#13215 = AXIS2_PLACEMENT_3D ( 'NONE', #5639, #14748, #10706 ) ;
#13216 = PLANE ( 'NONE',  #370 ) ;
#13217 = ADVANCED_FACE ( 'NONE', ( #18321 ), #11324, .F. ) ;
#13218 = EDGE_CURVE ( 'NONE', #17682, #5010, #14800, .T. ) ;
#13219 = ORIENTED_EDGE ( 'NONE', *, *, #8083, .F. ) ;
#13220 = UNCERTAINTY_MEASURE_WITH_UNIT (LENGTH_MEASURE( 1.000000000000000082E-05 ), #14442, 'distance_accuracy_value', 'NONE');
#13221 = LINE ( 'NONE', #17116, #16138 ) ;
#13222 = CARTESIAN_POINT ( 'NONE',  ( -89.48935565494650746, 89.10721938022165034, 51.64438126496267500 ) ) ;
#13223 = AXIS2_PLACEMENT_3D ( 'NONE', #15729, #11829, #3178 ) ;
#13225 = ORIENTED_EDGE ( 'NONE', *, *, #1761, .F. ) ;
#13224 = ORIENTED_EDGE ( 'NONE', *, *, #20185, .F. ) ;
#13226 = FACE_OUTER_BOUND ( 'NONE', #11605, .T. ) ;
#13227 = CARTESIAN_POINT ( 'NONE',  ( -52.87539273445160148, 109.4349703648165075, -43.48703773689284446 ) ) ;
#13228 = CARTESIAN_POINT ( 'NONE',  ( 16.39634482804422433, 187.9401017119210451, 319.7988598509798521 ) ) ;
#13229 = CARTESIAN_POINT ( 'NONE',  ( 4.169604791867612015, 166.7785703876306513, 322.5944574396354483 ) ) ;
#13230 = DIRECTION ( 'NONE',  ( 0.01292414190464133070, 0.000000000000000000, 0.9999164797902015955 ) ) ;
#13231 = ORIENTED_EDGE ( 'NONE', *, *, #11226, .T. ) ;
#13232 = VECTOR ( 'NONE', #4512, 1000.000000000000000 ) ;
#13233 = CARTESIAN_POINT ( 'NONE',  ( 106.8724933792760226, 79.04398536104964990, 26.04362031086705542 ) ) ;
#13234 = CARTESIAN_POINT ( 'NONE',  ( -12.64688860274155324, 109.6831087301383860, 124.2482791415423691 ) ) ;
#13235 = TOROIDAL_SURFACE ( 'NONE', #4016, 4.400000000000000355, 0.4000000000000000222 ) ;
#13236 = DIRECTION ( 'NONE',  ( 0.01292394549866740169, 0.005513023399720822990, 0.9999012842304693116 ) ) ;
#13237 = VERTEX_POINT ( 'NONE', #9728 ) ;
#13238 = DIRECTION ( 'NONE',  ( 0.000000000000000000, 1.000000000000000000, -0.000000000000000000 ) ) ;
#13239 = ORIENTED_EDGE ( 'NONE', *, *, #20498, .T. ) ;
#13240 = DIRECTION ( 'NONE',  ( -2.025474946048326158E-22, 1.000000000000000000, -1.876735158486679638E-22 ) ) ;
#13241 = DIRECTION ( 'NONE',  ( -0.000000000000000000, -1.000000000000000000, -0.000000000000000000 ) ) ;
#13242 = PRODUCT_DEFINITION_FORMATION_WITH_SPECIFIED_SOURCE ( 'ANY', '', #18549, .NOT_KNOWN. ) ;
#13243 = CARTESIAN_POINT ( 'NONE',  ( -10.91223172713801759, 137.6763543404365180, 122.9234154551231484 ) ) ;
#13244 = CARTESIAN_POINT ( 'NONE',  ( 45.44350069997230435, 168.6907664596095344, 34.02200722522286469 ) ) ;
#13245 = ORIENTED_EDGE ( 'NONE', *, *, #11390, .F. ) ;
#13246 = CARTESIAN_POINT ( 'NONE',  ( 64.99457118636311748, 169.9999999999999716, -0.8400692238016952418 ) ) ;
#13247 = CIRCLE ( 'NONE', #22, 4.374999999999991118 ) ;
#13248 = EDGE_LOOP ( 'NONE', ( #9753, #21822, #1604, #18026 ) ) ;
#13249 = DIRECTION ( 'NONE',  ( -0.6113012557851977835, -0.7913029548584309403, 0.01226410648014603956 ) ) ;
#13250 = EDGE_CURVE ( 'NONE', #10824, #13001, #6369, .T. ) ;
#13251 = CARTESIAN_POINT ( 'NONE',  ( -9.107733615807006800, 37.00000000000000711, -96.06569921463757566 ) ) ;
#13252 = ORIENTED_EDGE ( 'NONE', *, *, #3321, .T. ) ;
#13253 = AXIS2_PLACEMENT_3D ( 'NONE', #18188, #2440, #9430 ) ;
#13254 = VECTOR ( 'NONE', #17508, 1000.000000000000227 ) ;
#13255 = CARTESIAN_POINT ( 'NONE',  ( -88.16211553172512083, 88.11043810238577123, 53.02430440011134039 ) ) ;
#13256 = CARTESIAN_POINT ( 'NONE',  ( -88.82263333796718996, 169.9999999999999716, 1.148052203164670715 ) ) ;
#13257 = VERTEX_POINT ( 'NONE', #18450 ) ;
#13258 = AXIS2_PLACEMENT_3D ( 'NONE', #17557, #2261, #1809 ) ;
#13259 = DIRECTION ( 'NONE',  ( 0.000000000000000000, 0.000000000000000000, -1.000000000000000000 ) ) ;
#13260 = CARTESIAN_POINT ( 'NONE',  ( -4.863430190198783087, 189.4649401546927550, 275.2042792935563398 ) ) ;
#13261 = CARTESIAN_POINT ( 'NONE',  ( -10.75874152970787634, 105.7413430127404439, 134.7986624950468126 ) ) ;
#13262 = DIRECTION ( 'NONE',  ( 0.9999164797902017066, 6.965998958219365988E-18, -0.01292414190464157356 ) ) ;
#13263 = CARTESIAN_POINT ( 'NONE',  ( 41.59208321381912299, 69.99999999999998579, 84.46951292587608862 ) ) ;
#13264 = PRODUCT_DEFINITION ( 'UNKNOWN', '', #19809, #5789 ) ;
#13265 = CARTESIAN_POINT ( 'NONE',  ( 70.53865358177317546, 70.91952051830753589, 84.40563445996843939 ) ) ;
#13266 = ORIENTED_EDGE ( 'NONE', *, *, #14165, .F. ) ;
#13267 = DIRECTION ( 'NONE',  ( 0.9999164797902015955, 2.001050586450178695E-22, -0.01292414190464131335 ) ) ;
#13268 = CARTESIAN_POINT ( 'NONE',  ( 1.304573924809790730, 177.5566041281049081, 100.9324236879143371 ) ) ;
#13269 = CARTESIAN_POINT ( 'NONE',  ( 19.48840479045136576, 184.2293629865677929, 316.4953788918857640 ) ) ;
#13270 = CARTESIAN_POINT ( 'NONE',  ( 31.27336289421850424, 92.26071163157524779, -81.74815335747254608 ) ) ;
#13271 = AXIS2_PLACEMENT_3D ( 'NONE', #15372, #20626, #6612 ) ;
#13272 = DIRECTION ( 'NONE',  ( -0.01292414190464131335, -1.902755938799530239E-22, -0.9999164797902015955 ) ) ;
#13273 = CIRCLE ( 'NONE', #3344, 9.999999999999998224 ) ;
#13274 = AXIS2_PLACEMENT_3D ( 'NONE', #7961, #7861, #1084 ) ;
#13275 = CYLINDRICAL_SURFACE ( 'NONE', #42, 2.000000000000004441 ) ;
#13276 = CIRCLE ( 'NONE', #3350, 2.000000000000001776 ) ;
#13277 = CARTESIAN_POINT ( 'NONE',  ( -105.4334892372614121, 34.61572286322119396, 31.36525700924958926 ) ) ;
#13278 = ORIENTED_EDGE ( 'NONE', *, *, #11817, .T. ) ;
#13279 = LINE ( 'NONE', #9595, #18292 ) ;
#13280 = ORIENTED_EDGE ( 'NONE', *, *, #17423, .T. ) ;
#13281 = EDGE_CURVE ( 'NONE', #13983, #8794, #7689, .T. ) ;
#13282 = VERTEX_POINT ( 'NONE', #6390 ) ;
#13283 = CARTESIAN_POINT ( 'NONE',  ( 47.50856862875806286, 109.5708673988121262, -44.78527194220600904 ) ) ;
#13284 = DIRECTION ( 'NONE',  ( -0.9999164797902015955, -2.045733645417851681E-15, 0.01292414190464156835 ) ) ;
#13285 = VERTEX_POINT ( 'NONE', #22425 ) ;
#13286 = VERTEX_POINT ( 'NONE', #3251 ) ;
#13287 = CIRCLE ( 'NONE', #5914, 5.700000000000001954 ) ;
#13288 =( GEOMETRIC_REPRESENTATION_CONTEXT ( 3 ) GLOBAL_UNCERTAINTY_ASSIGNED_CONTEXT ( ( #2373 ) ) GLOBAL_UNIT_ASSIGNED_CONTEXT ( ( #4629, #4729, #13606 ) ) REPRESENTATION_CONTEXT ( 'NONE', 'WORKASPACE' ) );
#13289 = CARTESIAN_POINT ( 'NONE',  ( 93.23587179807657321, 72.00000000000000000, 30.79757858250317781 ) ) ;
#13290 = AXIS2_PLACEMENT_3D ( 'NONE', #21575, #704, #18175 ) ;
#13291 = CARTESIAN_POINT ( 'NONE',  ( -109.9781218937930447, 75.08416348859604739, -3.222660468417803514 ) ) ;
#13292 = ADVANCED_FACE ( 'NONE', ( #6598 ), #13623, .T. ) ;
#13293 = DIRECTION ( 'NONE',  ( 0.9909299940865190504, -0.1338359446631136318, -0.01207007604876911971 ) ) ;
#13294 = CARTESIAN_POINT ( 'NONE',  ( 0.000000000000000000, 25.00000000000000000, 0.000000000000000000 ) ) ;
#13295 = CIRCLE ( 'NONE', #3368, 2.000000000000001776 ) ;
#13296 = ORIENTED_EDGE ( 'NONE', *, *, #14162, .F. ) ;
#13297 = EDGE_CURVE ( 'NONE', #12076, #16780, #19206, .T. ) ;
#13298 = CARTESIAN_POINT ( 'NONE',  ( 13.25025589056750874, 189.1176631285997303, 275.3030354847988406 ) ) ;
#13299 = ORIENTED_EDGE ( 'NONE', *, *, #8342, .T. ) ;
#13300 = DIRECTION ( 'NONE',  ( 0.000000000000000000, 0.000000000000000000, -1.000000000000000000 ) ) ;
#13301 = CARTESIAN_POINT ( 'NONE',  ( 42.56450999050053952, 94.53367724843309361, 82.88992884652135729 ) ) ;
#13302 = CARTESIAN_POINT ( 'NONE',  ( 89.84434271629412194, 96.73102593143109118, -63.46658414958751848 ) ) ;
#13303 = CARTESIAN_POINT ( 'NONE',  ( -7.337194850064199692, 109.6999844229167564, 127.2409188565385421 ) ) ;
#13304 = EDGE_CURVE ( 'NONE', #14680, #7464, #5242, .T. ) ;
#13305 = CARTESIAN_POINT ( 'NONE',  ( 88.94497886703048550, 79.67058643966726095, -30.57398350459212821 ) ) ;
#13306 = FACE_OUTER_BOUND ( 'NONE', #7018, .T. ) ;
#13307 = VERTEX_POINT ( 'NONE', #11784 ) ;
#13308 = PLANE ( 'NONE',  #11811 ) ;
#13309 = VECTOR ( 'NONE', #6293, 1000.000000000000114 ) ;
#13310 = COLOUR_RGB ( '', 0.09019608, 0.27058824, 0.51372549) ;
#13311 = ORIENTED_EDGE ( 'NONE', *, *, #2493, .T. ) ;
#13312 = DIRECTION ( 'NONE',  ( -0.9999164797902017066, 0.000000000000000000, 0.01292414190463832269 ) ) ;
#13313 = CARTESIAN_POINT ( 'NONE',  ( -12.64734457064410478, 181.8784574882332379, 309.2558995593432769 ) ) ;
#13314 = ORIENTED_EDGE ( 'NONE', *, *, #106, .F. ) ;
#13315 = EDGE_CURVE ( 'NONE', #858, #1904, #11559, .T. ) ;
#13316 = VERTEX_POINT ( 'NONE', #9939 ) ;
#13317 = EDGE_CURVE ( 'NONE', #3464, #6883, #10470, .T. ) ;
#13318 = CIRCLE ( 'NONE', #1191, 4.999999999999994671 ) ;
#13319 = CARTESIAN_POINT ( 'NONE',  ( 163.9999999999998863, 20.00000000000000000, -8.000000000002268408 ) ) ;
#13320 = AXIS2_PLACEMENT_3D ( 'NONE', #14562, #11323, #2594 ) ;
#13321 = CIRCLE ( 'NONE', #14427, 6.499999999999998224 ) ;
#13322 = EDGE_CURVE ( 'NONE', #4610, #16423, #15936, .T. ) ;
#13323 = DIRECTION ( 'NONE',  ( -0.009760756503427893763, 0.9999378516499565217, -0.005387065077610108353 ) ) ;
#13324 = DIRECTION ( 'NONE',  ( -0.9770372205688160339, 0.2127605332646584080, 0.01145535281434409587 ) ) ;
#13325 = ORIENTED_EDGE ( 'NONE', *, *, #5269, .F. ) ;
#13326 = CARTESIAN_POINT ( 'NONE',  ( -41.45998972479013389, 170.2886526009413330, 277.1603356026176925 ) ) ;
#13327 = EDGE_CURVE ( 'NONE', #16446, #7377, #16671, .T. ) ;
#13328 = CARTESIAN_POINT ( 'NONE',  ( -13.52157056713759786, 180.8428797338423806, 308.0663627464555248 ) ) ;
#13329 = AXIS2_PLACEMENT_3D ( 'NONE', #20327, #11268, #14960 ) ;
#13330 = ORIENTED_EDGE ( 'NONE', *, *, #6496, .T. ) ;
#13331 = CARTESIAN_POINT ( 'NONE',  ( -59.30749807291185505, 114.2358014486931808, 170.6782526301398661 ) ) ;
#13332 = CARTESIAN_POINT ( 'NONE',  ( -38.50312546549035631, 96.48602976677958054, 84.62394436619374005 ) ) ;
#13333 = FACE_OUTER_BOUND ( 'NONE', #8819, .T. ) ;
#13334 = EDGE_LOOP ( 'NONE', ( #21124, #14384, #3371, #1194 ) ) ;
#13335 = CARTESIAN_POINT ( 'NONE',  ( -88.16117291386304089, 87.99029836822313655, 53.09774323446453081 ) ) ;
#13336 = VECTOR ( 'NONE', #6516, 1000.000000000000000 ) ;
#13337 = CARTESIAN_POINT ( 'NONE',  ( -9.888959084247115783, 187.7288727309014860, 308.1497221693155097 ) ) ;
#13338 = EDGE_CURVE ( 'NONE', #3438, #12198, #13726, .T. ) ;
#13339 = FACE_OUTER_BOUND ( 'NONE', #21448, .T. ) ;
#13340 = ORIENTED_EDGE ( 'NONE', *, *, #15289, .F. ) ;
#13341 = CARTESIAN_POINT ( 'NONE',  ( -39.99665919160808869, 170.0000000000000284, 0.5169656761856410432 ) ) ;
#13342 = DIRECTION ( 'NONE',  ( 7.125109674161246868E-05, -0.9999848031710253382, 0.005512562950850155054 ) ) ;
#13344 = VERTEX_POINT ( 'NONE', #19565 ) ;
#13343 = ORIENTED_EDGE ( 'NONE', *, *, #5623, .T. ) ;
#13345 = DIRECTION ( 'NONE',  ( 0.000000000000000000, 0.000000000000000000, -1.000000000000000000 ) ) ;
#13346 = CARTESIAN_POINT ( 'NONE',  ( -49.40977258443437137, 111.5098657627030434, -43.54327172089001152 ) ) ;
#13347 = CARTESIAN_POINT ( 'NONE',  ( 13.05740731942213095, 190.2969143928351059, 320.8495709388896557 ) ) ;
#13348 = PLANE ( 'NONE',  #4822 ) ;
#13349 = DIRECTION ( 'NONE',  ( 0.01292394549866733404, 0.005513023399720420534, 0.9999012842304693116 ) ) ;
#13350 = VECTOR ( 'NONE', #17547, 999.9999999999998863 ) ;
#13351 = DIRECTION ( 'NONE',  ( -0.01292394549866740169, -0.005513023399721021615, -0.9999012842304692006 ) ) ;
#13352 = TOROIDAL_SURFACE ( 'NONE', #161, 124.0000000000000000, 2.000000000000000000 ) ;
#13353 = CARTESIAN_POINT ( 'NONE',  ( -10.75931153848181054, 113.7412214381086670, 134.7545619914399992 ) ) ;
#13354 = LINE ( 'NONE', #8786, #7108 ) ;
#13355 = ORIENTED_EDGE ( 'NONE', *, *, #6148, .F. ) ;
#13356 = ADVANCED_FACE ( 'NONE', ( #176, #15929 ), #3601, .T. ) ;
#13357 = DIRECTION ( 'NONE',  ( -0.01292394549866740169, -0.005513023399721130903, -0.9999012842304692006 ) ) ;
#13358 = EDGE_LOOP ( 'NONE', ( #5774, #14648, #9062 ) ) ;
#13359 = CYLINDRICAL_SURFACE ( 'NONE', #19110, 8.000000000000003553 ) ;
#13360 = CARTESIAN_POINT ( 'NONE',  ( -1.089749515181836320E-13, 18.00000000000000355, 7.999999999999994671 ) ) ;
#13361 = CARTESIAN_POINT ( 'NONE',  ( 105.6848962833589809, 69.99999999999998579, 30.50771805806152770 ) ) ;
#13362 = DIRECTION ( 'NONE',  ( -0.9909299940865186063, 0.1338359446631179339, 0.01207007604875938098 ) ) ;
#13363 = CYLINDRICAL_SURFACE ( 'NONE', #18111, 2.000000000000001776 ) ;
#13364 = CARTESIAN_POINT ( 'NONE',  ( -50.90866737042907175, 114.2432658504114613, 170.0089255777808432 ) ) ;
#13365 = CIRCLE ( 'NONE', #3433, 3.399999999999991918 ) ;
#13366 = ORIENTED_EDGE ( 'NONE', *, *, #21534, .T. ) ;
#13367 = DIRECTION ( 'NONE',  ( -0.000000000000000000, -0.000000000000000000, -1.000000000000000000 ) ) ;
#13368 = ADVANCED_FACE ( 'NONE', ( #14312 ), #15807, .T. ) ;
#13369 = CARTESIAN_POINT ( 'NONE',  ( -41.00865927789263310, 166.2639521169525665, 308.9298270502609967 ) ) ;
#13370 = ORIENTED_EDGE ( 'NONE', *, *, #20170, .T. ) ;
#13371 = VECTOR ( 'NONE', #4837, 1000.000000000000227 ) ;
#13372 = ORIENTED_EDGE ( 'NONE', *, *, #6553, .T. ) ;
#13373 = AXIS2_PLACEMENT_3D ( 'NONE', #19274, #7321, #108 ) ;
#13374 = CARTESIAN_POINT ( 'NONE',  ( -89.99511487588330283, 88.72984820209772749, 52.48309319825106201 ) ) ;
#13375 = LINE ( 'NONE', #856, #16320 ) ;
#13376 = ORIENTED_EDGE ( 'NONE', *, *, #6650, .T. ) ;
#13377 = VERTEX_POINT ( 'NONE', #2009 ) ;
#13378 = DIRECTION ( 'NONE',  ( 0.000000000000000000, -1.000000000000000000, 0.000000000000000000 ) ) ;
#13379 = CIRCLE ( 'NONE', #6400, 2.000000000000001332 ) ;
#13380 = DIRECTION ( 'NONE',  ( 0.7098319280015313870, -0.09073800780701757329, 0.6985021459729685578 ) ) ;
#13381 = DIRECTION ( 'NONE',  ( -5.440186201345738641E-18, -1.000000000000000000, -1.334940939666364181E-17 ) ) ;
#13382 = LINE ( 'NONE', #15555, #19009 ) ;
#13383 = FACE_OUTER_BOUND ( 'NONE', #18750, .T. ) ;
#13384 = ADVANCED_FACE ( 'NONE', ( #14084 ), #1554, .F. ) ;
#13385 = ORIENTED_EDGE ( 'NONE', *, *, #2712, .F. ) ;
#13386 = EDGE_CURVE ( 'NONE', #9075, #5608, #7052, .T. ) ;
#13387 = CARTESIAN_POINT ( 'NONE',  ( 48.58946335778052372, 189.4003865961453812, -109.4536762928195230 ) ) ;
#13388 = CARTESIAN_POINT ( 'NONE',  ( 8.732865712828665750, 190.3249964942741883, 274.4707185275763095 ) ) ;
#13389 = CARTESIAN_POINT ( 'NONE',  ( 19.91815129952728469, 182.7044225173947893, 313.0591062094031258 ) ) ;
#13390 = TOROIDAL_SURFACE ( 'NONE', #13738, 8.000000000000014211, 2.000000000000000000 ) ;
#13391 = CARTESIAN_POINT ( 'NONE',  ( -90.02465904577691447, 70.02851260093143537, 63.21045060945284888 ) ) ;
#13392 = VECTOR ( 'NONE', #4523, 1000.000000000000114 ) ;
#13393 = CARTESIAN_POINT ( 'NONE',  ( -5.727992348863838679, 144.0418861141313300, 276.6809104038102305 ) ) ;
#13394 = EDGE_LOOP ( 'NONE', ( #3566, #7889, #6998, #2040, #11659, #21957, #13851, #21249, #21619, #7157, #18181, #5395, #5910, #8198, #15658, #684, #15802, #6230, #7583, #17428, #21772, #8913 ) ) ;
#13395 = DIRECTION ( 'NONE',  ( 0.000000000000000000, 0.000000000000000000, 1.000000000000000000 ) ) ;
#13396 = DIRECTION ( 'NONE',  ( 0.01292394549866740169, 0.005513023399720822990, 0.9999012842304693116 ) ) ;
#13397 = CARTESIAN_POINT ( 'NONE',  ( -41.41899454747574083, 166.0889136240115249, 277.1829612759436827 ) ) ;
#13398 = CARTESIAN_POINT ( 'NONE',  ( -10.85283309178001687, 186.7056505379215139, 320.9993531894351122 ) ) ;
#13399 = ORIENTED_EDGE ( 'NONE', *, *, #5863, .T. ) ;
#13400 = AXIS2_PLACEMENT_3D ( 'NONE', #19260, #20752, #5006 ) ;
#13401 = CARTESIAN_POINT ( 'NONE',  ( -14.44752122961171104, 185.3991216854906838, 276.7278808722562076 ) ) ;
#13402 = EDGE_LOOP ( 'NONE', ( #10118, #19216, #9885, #21589 ) ) ;
#13403 = CARTESIAN_POINT ( 'NONE',  ( 41.32205096979155456, 107.3883277703369288, 70.91984598015065444 ) ) ;
#13404 = TOROIDAL_SURFACE ( 'NONE', #4205, 10.00000000000000355, 2.000000000000000000 ) ;
#13405 = ORIENTED_EDGE ( 'NONE', *, *, #18930, .T. ) ;
#13406 = CARTESIAN_POINT ( 'NONE',  ( -49.09819033004664846, 107.9573722685052388, 70.09443008244173257 ) ) ;
#13407 = CARTESIAN_POINT ( 'NONE',  ( 9.196690372329060281, 142.8086146031528187, 274.7267082784170498 ) ) ;
#13408 = CARTESIAN_POINT ( 'NONE',  ( 105.8709953322713488, 79.07548657612767329, -29.85559726770835098 ) ) ;
#13409 = ADVANCED_FACE ( 'NONE', ( #13843 ), #6822, .T. ) ;
#13410 = CARTESIAN_POINT ( 'NONE',  ( -93.18852247616528928, 70.03011042807717956, -58.44685241948167231 ) ) ;
#13411 = CARTESIAN_POINT ( 'NONE',  ( 19.93803444517712720, 184.4413408268273429, 278.2191123044462984 ) ) ;
#13412 = CARTESIAN_POINT ( 'NONE',  ( -55.33623483430230294, 88.81971041278778500, 167.7780138627090025 ) ) ;
#13413 = CARTESIAN_POINT ( 'NONE',  ( 6.254127940454616841, 81.99999999999998579, -84.87602797277141065 ) ) ;
#13414 = AXIS2_PLACEMENT_3D ( 'NONE', #16915, #4600, #16803 ) ;
#13415 = CARTESIAN_POINT ( 'NONE',  ( 49.99582398951007889, 170.0000000000000284, -0.6462070952321007367 ) ) ;
#13416 = CARTESIAN_POINT ( 'NONE',  ( -54.68979215835705077, 114.2467007792763098, 172.5957179600166569 ) ) ;
#13417 = CYLINDRICAL_SURFACE ( 'NONE', #14357, 83.99999999999998579 ) ;
#13418 = ORIENTED_EDGE ( 'NONE', *, *, #17363, .F. ) ;
#13419 = CARTESIAN_POINT ( 'NONE',  ( 93.38631075262973980, 69.99999999999998579, 58.13036983636535382 ) ) ;
#13420 = ORIENTED_EDGE ( 'NONE', *, *, #12322, .F. ) ;
#13421 = CARTESIAN_POINT ( 'NONE',  ( 84.07537730384214569, 105.0000000000000000, 70.09082476868245237 ) ) ;
#13422 = CARTESIAN_POINT ( 'NONE',  ( -12.18818533274768967, 185.3912375219357500, 308.8328755857670558 ) ) ;
#13423 = ORIENTED_EDGE ( 'NONE', *, *, #15008, .T. ) ;
#13424 = ORIENTED_EDGE ( 'NONE', *, *, #11289, .F. ) ;
#13425 = PRESENTATION_LAYER_ASSIGNMENT (  '', '', ( #3118 ) ) ;
#13426 = CARTESIAN_POINT ( 'NONE',  ( -68.58360120290727480, 71.33040186743640731, 86.00170974875814522 ) ) ;
#13427 = ORIENTED_EDGE ( 'NONE', *, *, #3791, .T. ) ;
#13428 = FACE_OUTER_BOUND ( 'NONE', #8609, .T. ) ;
#13429 = DIRECTION ( 'NONE',  ( 0.000000000000000000, -0.005512562964840580192, -0.9999848057093461140 ) ) ;
#13430 = FACE_BOUND ( 'NONE', #17268, .T. ) ;
#13431 = EDGE_CURVE ( 'NONE', #11828, #379, #2336, .T. ) ;
#13432 = ORIENTED_EDGE ( 'NONE', *, *, #15533, .T. ) ;
#13433 = ADVANCED_FACE ( 'NONE', ( #12358 ), #17765, .F. ) ;
#13434 = CARTESIAN_POINT ( 'NONE',  ( -14.50562271935455172, 179.3719498139292341, 319.5410565726744494 ) ) ;
#13435 = CARTESIAN_POINT ( 'NONE',  ( -60.04913677256507754, 114.3120678458336812, 169.7095331739204767 ) ) ;
#13437 = CARTESIAN_POINT ( 'NONE',  ( 0.000000000000000000, 37.00000000000000711, 0.000000000000000000 ) ) ;
#13436 = CARTESIAN_POINT ( 'NONE',  ( -37.43179216281937016, 95.93806238594169145, 85.10200020414913524 ) ) ;
#13438 = AXIS2_PLACEMENT_3D ( 'NONE', #16899, #1390, #14857 ) ;
#13439 = CYLINDRICAL_SURFACE ( 'NONE', #9971, 2.000000000000004885 ) ;
#13440 = ORIENTED_EDGE ( 'NONE', *, *, #22227, .T. ) ;
#13441 = CARTESIAN_POINT ( 'NONE',  ( 59.68254426988709582, 143.9326556260109555, 168.4877485356595912 ) ) ;
#13442 = DIRECTION ( 'NONE',  ( -0.01292394549866632963, -0.005513023399716958026, -0.9999012842304692006 ) ) ;
#13443 = CARTESIAN_POINT ( 'NONE',  ( 17.94009145739756050, 145.7869293583445938, 276.2000847856109544 ) ) ;
#13444 = CARTESIAN_POINT ( 'NONE',  ( -24.25006591444867965, 324.5132455039467345, 307.8723024395048355 ) ) ;
#13445 = EDGE_CURVE ( 'NONE', #5068, #16242, #8928, .T. ) ;
#13446 = ADVANCED_FACE ( 'NONE', ( #19107 ), #21067, .F. ) ;
#13447 = ORIENTED_EDGE ( 'NONE', *, *, #16308, .F. ) ;
#13448 = LINE ( 'NONE', #7918, #9509 ) ;
#13449 = CARTESIAN_POINT ( 'NONE',  ( -90.03465221005033925, 70.01281497139055432, 63.19621350536183968 ) ) ;
#13450 = EDGE_CURVE ( 'NONE', #495, #21379, #7095, .T. ) ;
#13451 = CONTEXT_DEPENDENT_SHAPE_REPRESENTATION ( #10871, #22194 ) ;
#13452 = EDGE_LOOP ( 'NONE', ( #20260, #3851 ) ) ;
#13453 = CARTESIAN_POINT ( 'NONE',  ( -52.31042862874694777, 111.8905520295979983, -46.77079012771374522 ) ) ;
#13454 = ORIENTED_EDGE ( 'NONE', *, *, #17504, .F. ) ;
#13455 = PLANE ( 'NONE',  #1505 ) ;
#13456 = CARTESIAN_POINT ( 'NONE',  ( -10.95260071218788767, 105.6586476617446380, 119.8001432315898001 ) ) ;
#13457 = CARTESIAN_POINT ( 'NONE',  ( 4.182528737366220106, 166.7840834110302808, 323.5943587238651276 ) ) ;
#13458 = LINE ( 'NONE', #11505, #19668 ) ;
#13459 = CARTESIAN_POINT ( 'NONE',  ( 88.82263333796723259, 169.9999999999999716, -1.148052203164690033 ) ) ;
#13460 = ORIENTED_EDGE ( 'NONE', *, *, #15442, .F. ) ;
#13461 = ADVANCED_FACE ( 'NONE', ( #8997 ), #21280, .T. ) ;
#13462 = CARTESIAN_POINT ( 'NONE',  ( -72.51438462527775641, 87.23323244114081376, 69.92599951943640235 ) ) ;
#13463 = DIRECTION ( 'NONE',  ( -0.01292394549866695240, -0.005513023399725255208, -0.9999012842304693116 ) ) ;
#13464 = ORIENTED_EDGE ( 'NONE', *, *, #9901, .F. ) ;
#13465 = CARTESIAN_POINT ( 'NONE',  ( -42.56628114047011735, 94.99786382055523859, -43.54068532293076288 ) ) ;
#13466 = DIRECTION ( 'NONE',  ( 0.01292414190464044946, 1.902755938799528828E-22, 0.9999164797902017066 ) ) ;
#13467 = DIRECTION ( 'NONE',  ( 0.01292414190464131335, 0.000000000000000000, 0.9999164797902017066 ) ) ;
#13468 = DIRECTION ( 'NONE',  ( -0.01292394549866739996, -0.005513023399721131770, -0.9999012842304692006 ) ) ;
#13469 = ADVANCED_FACE ( 'NONE', ( #279, #22632 ), #5206, .F. ) ;
#13470 = VERTEX_POINT ( 'NONE', #18302 ) ;
#13471 = DIRECTION ( 'NONE',  ( -1.000000000000000000, 0.000000000000000000, -1.372099599554301422E-14 ) ) ;
#13472 = ORIENTED_EDGE ( 'NONE', *, *, #2190, .T. ) ;
#13473 = CARTESIAN_POINT ( 'NONE',  ( 47.42620204064805023, 94.99786382055523859, -44.70385809434849733 ) ) ;
#13474 = DIRECTION ( 'NONE',  ( 0.01292414190464125957, 0.000000000000000000, 0.9999164797902015955 ) ) ;
#13475 = EDGE_LOOP ( 'NONE', ( #12236, #12225 ) ) ;
#13476 = LINE ( 'NONE', #1063, #3617 ) ;
#13477 = CARTESIAN_POINT ( 'NONE',  ( -90.07216641000893276, 88.57119983275795505, 52.67302757455067308 ) ) ;
#13478 = ADVANCED_FACE ( 'NONE', ( #13147 ), #16487, .F. ) ;
#13479 = ORIENTED_EDGE ( 'NONE', *, *, #22366, .F. ) ;
#13480 = CARTESIAN_POINT ( 'NONE',  ( -75.30975508861040169, 94.90914755154933857, 80.17755788556743823 ) ) ;
#13481 = CARTESIAN_POINT ( 'NONE',  ( -38.21549050681395698, 167.4026153394593734, 273.1339171915171846 ) ) ;
#13482 = DIRECTION ( 'NONE',  ( -0.01292394549866731843, -0.005513023399720594006, -0.9999012842304693116 ) ) ;
#13483 = EDGE_LOOP ( 'NONE', ( #7867, #12707, #20123, #621, #7327, #9654 ) ) ;
#13484 = LINE ( 'NONE', #18005, #841 ) ;
#13485 = CARTESIAN_POINT ( 'NONE',  ( 51.42455095033975709, 113.4816418249608034, -44.85744920025983618 ) ) ;
#13486 = AXIS2_PLACEMENT_3D ( 'NONE', #228, #20776, #2628 ) ;
#13487 = CARTESIAN_POINT ( 'NONE',  ( -71.26616241777601601, 92.22173151023517335, -83.79227730723270895 ) ) ;
#13488 = EDGE_CURVE ( 'NONE', #22420, #8988, #19920, .T. ) ;
#13489 = VERTEX_POINT ( 'NONE', #10954 ) ;
#13490 = ADVANCED_BREP_SHAPE_REPRESENTATION ( '', ( #17529, #6292 ), #18057 ) ;
#13491 = VERTEX_POINT ( 'NONE', #21396 ) ;
#13492 = CARTESIAN_POINT ( 'NONE',  ( -109.6363981638670566, 79.04398536104955042, 28.84204567386034057 ) ) ;
#13493 = CARTESIAN_POINT ( 'NONE',  ( 44.62344841673415630, 166.7281037598372961, 233.8131482778615577 ) ) ;
#13494 = CARTESIAN_POINT ( 'NONE',  ( 146.4999999999998579, 2.000000000000000000, 9.999999999997978506 ) ) ;
#13495 = DIRECTION ( 'NONE',  ( 7.125109674403277385E-05, -0.9999848031710253382, 0.005512562950848281552 ) ) ;
#13496 = CARTESIAN_POINT ( 'NONE',  ( -9.607300630488882831, 146.1747715025532557, 278.1621700325267739 ) ) ;
#13497 = CARTESIAN_POINT ( 'NONE',  ( 79.99331838321626265, 102.0000000000000000, -1.033931352371318058 ) ) ;
#13498 = VERTEX_POINT ( 'NONE', #18207 ) ;
#13499 = CARTESIAN_POINT ( 'NONE',  ( -5.929909278051283650, 37.00000000000000711, -93.63641280122985222 ) ) ;
#13500 = EDGE_LOOP ( 'NONE', ( #1424, #10875 ) ) ;
#13501 = ORIENTED_EDGE ( 'NONE', *, *, #11205, .T. ) ;
#13502 = ORIENTED_EDGE ( 'NONE', *, *, #9466, .F. ) ;
#13503 = CIRCLE ( 'NONE', #17918, 6.000000000000004441 ) ;
#13504 = CARTESIAN_POINT ( 'NONE',  ( -51.19750717848778265, 189.4876967392748384, -92.32575444861939218 ) ) ;
#13505 = EDGE_CURVE ( 'NONE', #251, #2761, #9361, .T. ) ;
#13506 = EDGE_CURVE ( 'NONE', #7858, #16531, #17379, .T. ) ;
#13507 = ORIENTED_EDGE ( 'NONE', *, *, #12756, .F. ) ;
#13508 = CARTESIAN_POINT ( 'NONE',  ( -49.19269645916414646, 107.6774848903028072, 70.52757125197122434 ) ) ;
#13509 = CARTESIAN_POINT ( 'NONE',  ( 42.75298547076369715, 108.3652131041115467, 57.98564716923558393 ) ) ;
#13510 = CARTESIAN_POINT ( 'NONE',  ( 83.18996550559461411, 75.15486823347328027, 4.352207832899844142 ) ) ;
#13511 = DIRECTION ( 'NONE',  ( -0.9999164797902015955, -6.965998958219364448E-18, 0.01292414190464157182 ) ) ;
#13512 = CARTESIAN_POINT ( 'NONE',  ( 18.81027419078025176, 185.4549478099342252, 276.6073258177660819 ) ) ;
#13513 =( NAMED_UNIT ( * ) PLANE_ANGLE_UNIT ( ) SI_UNIT ( $, .RADIAN. ) );
#13514 = DIRECTION ( 'NONE',  ( -0.01292394549866695240, -0.005513023399718316314, -0.9999012842304693116 ) ) ;
#13515 = DIRECTION ( 'NONE',  ( 0.01292394549866738782, 0.005513023399720468239, 0.9999012842304692006 ) ) ;
#13516 = CARTESIAN_POINT ( 'NONE',  ( -7.337194850064199692, 109.6999844229167564, 127.2409188565385421 ) ) ;
#13517 = CIRCLE ( 'NONE', #19000, 85.00000000000002842 ) ;
#13518 = CARTESIAN_POINT ( 'NONE',  ( 88.55041925573031847, 79.97987315375630146, -31.50236046386200428 ) ) ;
#13519 = EDGE_LOOP ( 'NONE', ( #3658, #7008, #6920, #5423 ) ) ;
#13520 = CARTESIAN_POINT ( 'NONE',  ( 0.000000000000000000, 23.00000000000000000, 118.0000000000000000 ) ) ;
#13521 = VERTEX_POINT ( 'NONE', #2569 ) ;
#13522 = ORIENTED_EDGE ( 'NONE', *, *, #15604, .F. ) ;
#13523 = LINE ( 'NONE', #3395, #14727 ) ;
#13524 = CARTESIAN_POINT ( 'NONE',  ( -55.40268456415262932, 18.00000000000000355, 113.1659955246495883 ) ) ;
#13525 = ORIENTED_EDGE ( 'NONE', *, *, #20579, .F. ) ;
#13526 = FACE_OUTER_BOUND ( 'NONE', #3772, .T. ) ;
#13527 = VECTOR ( 'NONE', #10865, 1000.000000000000000 ) ;
#13528 = ORIENTED_EDGE ( 'NONE', *, *, #4413, .F. ) ;
#13529 = EDGE_CURVE ( 'NONE', #4193, #18705, #20712, .T. ) ;
#13530 =( GEOMETRIC_REPRESENTATION_CONTEXT ( 3 ) GLOBAL_UNCERTAINTY_ASSIGNED_CONTEXT ( ( #12454 ) ) GLOBAL_UNIT_ASSIGNED_CONTEXT ( ( #3037, #8096, #9825 ) ) REPRESENTATION_CONTEXT ( 'NONE', 'WORKASPACE' ) );
#13531 =( REPRESENTATION_RELATIONSHIP ('NONE','NONE', #11808, #15634 ) REPRESENTATION_RELATIONSHIP_WITH_TRANSFORMATION ( #15626 )SHAPE_REPRESENTATION_RELATIONSHIP( ) );
#13532 = CARTESIAN_POINT ( 'NONE',  ( -66.18268079339598842, 69.99999999999998579, 87.86269266872857031 ) ) ;
#13533 = DIRECTION ( 'NONE',  ( 0.01292394549866737741, 0.005513023399721125699, 0.9999012842304693116 ) ) ;
#13534 = CARTESIAN_POINT ( 'NONE',  ( -9.804288294571927409, 187.7022783261437837, 321.1616740932373091 ) ) ;
#13535 = CARTESIAN_POINT ( 'NONE',  ( 14.49661276311460334, 144.7736480898878426, 276.2294396764298767 ) ) ;
#13536 = DIRECTION ( 'NONE',  ( 0.01292394549866727853, 0.005513023399720741458, 0.9999012842304692006 ) ) ;
#13537 = CIRCLE ( 'NONE', #10591, 2.000000000000004885 ) ;
#13538 = CYLINDRICAL_SURFACE ( 'NONE', #17623, 112.5000000000000284 ) ;
#13539 = CARTESIAN_POINT ( 'NONE',  ( 109.5443584724616670, 75.69229587323870589, 10.26624083857056569 ) ) ;
#13540 = CIRCLE ( 'NONE', #19391, 4.500000000000006217 ) ;
#13541 = CARTESIAN_POINT ( 'NONE',  ( 8.492591494844878852, 70.35931727281543147, -90.21500375438166941 ) ) ;
#13542 = ORIENTED_EDGE ( 'NONE', *, *, #3620, .F. ) ;
#13543 = DIRECTION ( 'NONE',  ( 0.000000000000000000, -0.000000000000000000, 1.000000000000000000 ) ) ;
#13544 = DIRECTION ( 'NONE',  ( 0.9999464000778708339, 1.417269118681874529E-05, -0.01035358732233823860 ) ) ;
#13545 = DIRECTION ( 'NONE',  ( 7.125109674160325297E-05, -0.9999848031710252272, 0.005512562950849327591 ) ) ;
#13546 = LINE ( 'NONE', #8459, #19457 ) ;
#13547 = CARTESIAN_POINT ( 'NONE',  ( -28.36560386230606667, 324.0744542294598887, 315.7670840739926916 ) ) ;
#13548 = AXIS2_PLACEMENT_3D ( 'NONE', #2533, #14852, #934 ) ;
#13549 = ADVANCED_FACE ( 'NONE', ( #16155 ), #17511, .T. ) ;
#13550 = DIRECTION ( 'NONE',  ( -1.000000000000000000, 0.000000000000000000, 9.912705577010318154E-17 ) ) ;
#13551 = CARTESIAN_POINT ( 'NONE',  ( 41.09521125350256909, 91.17157287525387233, 84.47593510598149180 ) ) ;
#13552 = PRODUCT_CONTEXT ( 'NONE', #21842, 'mechanical' ) ;
#13553 = ADVANCED_FACE ( 'NONE', ( #21608 ), #2111, .T. ) ;
#13554 = VERTEX_POINT ( 'NONE', #18099 ) ;
#13555 = CARTESIAN_POINT ( 'NONE',  ( -154.0000000000000000, 20.00000000000000000, 53.76161406891259986 ) ) ;
#13556 = CARTESIAN_POINT ( 'NONE',  ( 14.26054767869631945, 189.5762264811534692, 320.6589299877209669 ) ) ;
#13557 = LINE ( 'NONE', #3192, #17701 ) ;
#13558 = DIRECTION ( 'NONE',  ( -0.9999464000778710560, -1.417269118681194361E-05, 0.01035358732233947372 ) ) ;
#13559 = ORIENTED_EDGE ( 'NONE', *, *, #9376, .F. ) ;
#13560 = CARTESIAN_POINT ( 'NONE',  ( -45.67439959886510081, 164.8106407359766763, -51.88621947793163258 ) ) ;
#13561 = CYLINDRICAL_SURFACE ( 'NONE', #13003, 1.999999999999997780 ) ;
#13562 = EDGE_CURVE ( 'NONE', #369, #367, #9057, .T. ) ;
#13563 = ORIENTED_EDGE ( 'NONE', *, *, #10185, .F. ) ;
#13564 = CARTESIAN_POINT ( 'NONE',  ( -88.44870386694205422, 88.71936310223436806, 50.32514765335821494 ) ) ;
#13565 = ORIENTED_EDGE ( 'NONE', *, *, #19607, .T. ) ;
#13566 =( LENGTH_UNIT ( ) NAMED_UNIT ( * ) SI_UNIT ( .MILLI., .METRE. ) );
#13567 = ADVANCED_FACE ( 'NONE', ( #6687 ), #10032, .T. ) ;
#13568 = DIRECTION ( 'NONE',  ( 0.7161863329816273716, 0.003898296230782334528, 0.6978982302147116457 ) ) ;
#13569 = CARTESIAN_POINT ( 'NONE',  ( 0.000000000000000000, 25.00000000000000000, 0.000000000000000000 ) ) ;
#13570 = DIRECTION ( 'NONE',  ( -7.125109674364536131E-05, 0.9999848031710253382, -0.005512562950849705760 ) ) ;
#13571 = VECTOR ( 'NONE', #9018, 999.9999999999998863 ) ;
#13572 = AXIS2_PLACEMENT_3D ( 'NONE', #17384, #8321, #13300 ) ;
#13573 = EDGE_CURVE ( 'NONE', #19957, #251, #17053, .T. ) ;
#13574 = FACE_OUTER_BOUND ( 'NONE', #20740, .T. ) ;
#13575 = VECTOR ( 'NONE', #8799, 1000.000000000000114 ) ;
#13576 = EDGE_LOOP ( 'NONE', ( #4805, #7182, #11164, #6489 ) ) ;
#13577 = DIRECTION ( 'NONE',  ( -0.9999164797902015955, -2.001050586450178695E-22, 0.01292414190464131335 ) ) ;
#13578 = CARTESIAN_POINT ( 'NONE',  ( 79.99331838321626265, 55.99999999999999289, -1.033931352371318058 ) ) ;
#13579 = ORIENTED_EDGE ( 'NONE', *, *, #10972, .T. ) ;
#13580 = ADVANCED_FACE ( 'NONE', ( #8296 ), #1973, .F. ) ;
#13581 = CARTESIAN_POINT ( 'NONE',  ( -64.15090010559214306, 90.56097911118510524, 66.11330928953715613 ) ) ;
#13582 = CARTESIAN_POINT ( 'NONE',  ( -90.12303247369654002, 87.40561052298997424, 51.15152651009733376 ) ) ;
#13583 = EDGE_CURVE ( 'NONE', #899, #19083, #20358, .T. ) ;
#13584 = AXIS2_PLACEMENT_3D ( 'NONE', #14713, #22450, #3073 ) ;
#13585 = VERTEX_POINT ( 'NONE', #1420 ) ;
#13586 = AXIS2_PLACEMENT_3D ( 'NONE', #11646, #8073, #20465 ) ;
#13587 = DIRECTION ( 'NONE',  ( 0.000000000000000000, 0.000000000000000000, -1.000000000000000000 ) ) ;
#13588 = CARTESIAN_POINT ( 'NONE',  ( -33.82085273160089400, 93.50464841319747222, 82.93470554904384073 ) ) ;
#13589 = FACE_OUTER_BOUND ( 'NONE', #19978, .T. ) ;
#13590 = EDGE_LOOP ( 'NONE', ( #14058, #8090, #17844, #1088, #21963 ) ) ;
#13591 = AXIS2_PLACEMENT_3D ( 'NONE', #7882, #21861, #5796 ) ;
#13592 =( LENGTH_UNIT ( ) NAMED_UNIT ( * ) SI_UNIT ( .MILLI., .METRE. ) );
#13593 = CARTESIAN_POINT ( 'NONE',  ( -90.43417961988758691, 79.20545292891345923, 29.12427242046052456 ) ) ;
#13594 = LINE ( 'NONE', #15333, #15934 ) ;
#13595 = EDGE_CURVE ( 'NONE', #12084, #18692, #6362, .T. ) ;
#13596 = CONICAL_SURFACE ( 'NONE', #21625, 3.047499999999998987, 1.047197551196594523 ) ;
#13597 = ORIENTED_EDGE ( 'NONE', *, *, #1984, .F. ) ;
#13598 = DIRECTION ( 'NONE',  ( 0.9999164797902017066, 0.000000000000000000, -0.01292414190464174703 ) ) ;
#13599 = CARTESIAN_POINT ( 'NONE',  ( -3.468421381707180728, 158.8820161015420354, 323.7368175311311802 ) ) ;
#13600 = DIRECTION ( 'NONE',  ( 5.257943380984030796E-16, -1.000000000000000000, -6.795817950787834712E-18 ) ) ;
#13601 = EDGE_CURVE ( 'NONE', #11233, #18558, #5632, .T. ) ;
#13602 = DIRECTION ( 'NONE',  ( -0.9250486434174662875, -0.3795887553195633202, 0.01404934683357507604 ) ) ;
#13603 = CARTESIAN_POINT ( 'NONE',  ( 4.150218873619610171, 166.7703008525310793, 321.0946055132897072 ) ) ;
#13604 = EDGE_CURVE ( 'NONE', #3576, #20464, #22396, .T. ) ;
#13605 = ORIENTED_EDGE ( 'NONE', *, *, #3728, .T. ) ;
#13606 =( NAMED_UNIT ( * ) SI_UNIT ( $, .STERADIAN. ) SOLID_ANGLE_UNIT ( ) );
#13607 = CIRCLE ( 'NONE', #14720, 3.100000000000005418 ) ;
#13608 = PRODUCT_DEFINITION_SHAPE ( 'NONE', 'NONE',  #22687 ) ;
#13609 = VECTOR ( 'NONE', #15621, 999.9999999999998863 ) ;
#13610 = CIRCLE ( 'NONE', #18371, 95.00000000000004263 ) ;
#13611 = DIRECTION ( 'NONE',  ( -0.009760756503428008254, 0.9999378516499565217, -0.005387065077611300108 ) ) ;
#13612 = VERTEX_POINT ( 'NONE', #1201 ) ;
#13613 = AXIS2_PLACEMENT_3D ( 'NONE', #19808, #7544, #4196 ) ;
#13614 = CARTESIAN_POINT ( 'NONE',  ( -11.79420393680612023, 185.2698227558952624, 278.4462014808021308 ) ) ;
#13615 = ORIENTED_EDGE ( 'NONE', *, *, #16410, .F. ) ;
#13616 = CARTESIAN_POINT ( 'NONE',  ( -18.97922986118555500, 97.26594046717956132, 79.10430693329942642 ) ) ;
#13617 = EDGE_CURVE ( 'NONE', #11404, #21601, #3579, .T. ) ;
#13618 = AXIS2_PLACEMENT_3D ( 'NONE', #1246, #3505, #8234 ) ;
#13619 = ORIENTED_EDGE ( 'NONE', *, *, #3011, .T. ) ;
#13620 = DIRECTION ( 'NONE',  ( 0.01246513159389405628, 0.2641402835564741203, 0.9644037178988125181 ) ) ;
#13621 = CARTESIAN_POINT ( 'NONE',  ( -85.63433794141032251, 105.0000000000000000, -69.04172771111927887 ) ) ;
#13622 = AXIS2_PLACEMENT_3D ( 'NONE', #9325, #8257, #13543 ) ;
#13623 = CYLINDRICAL_SURFACE ( 'NONE', #11524, 110.5324305509042233 ) ;
#13624 = VECTOR ( 'NONE', #7751, 1000.000000000000114 ) ;
#13625 = PLANE ( 'NONE',  #15918 ) ;
#13626 = CARTESIAN_POINT ( 'NONE',  ( -41.34578887370003031, 158.5893797366368290, 277.2233642640256903 ) ) ;
#13627 = ORIENTED_EDGE ( 'NONE', *, *, #2259, .T. ) ;
#13628 = CARTESIAN_POINT ( 'NONE',  ( 16.40873467035000033, 185.6567299720572635, 322.3321779654820602 ) ) ;
#13629 = CARTESIAN_POINT ( 'NONE',  ( 13.03253886790000315, 190.3482298048060386, 320.8504275187944472 ) ) ;
#13630 = CARTESIAN_POINT ( 'NONE',  ( -41.59208321381909457, 72.00000000000000000, -84.46951292587610283 ) ) ;
#13631 = CARTESIAN_POINT ( 'NONE',  ( -1.124400345703740589, 69.99999999999998579, -86.99273374174759965 ) ) ;
#13632 = DIRECTION ( 'NONE',  ( -2.025474946048326158E-22, 1.000000000000000000, -1.876735158486679638E-22 ) ) ;
#13633 = EDGE_CURVE ( 'NONE', #19439, #5742, #18537, .T. ) ;
#13634 = ORIENTED_EDGE ( 'NONE', *, *, #19061, .F. ) ;
#13635 = CIRCLE ( 'NONE', #2233, 3.047499999999988329 ) ;
#13636 = CARTESIAN_POINT ( 'NONE',  ( -71.83229293602242649, 94.61330589943089819, 83.32202392072876762 ) ) ;
#13637 = VERTEX_POINT ( 'NONE', #14988 ) ;
#13638 = EDGE_LOOP ( 'NONE', ( #11978, #9408 ) ) ;
#13639 = CARTESIAN_POINT ( 'NONE',  ( -38.72625626464041915, 94.79963607512176793, 84.18062813568484160 ) ) ;
#13640 = CARTESIAN_POINT ( 'NONE',  ( 39.39497909003009823, 69.99999999999998579, -85.51628863845822082 ) ) ;
#13641 = ORIENTED_EDGE ( 'NONE', *, *, #18112, .T. ) ;
#13642 = CARTESIAN_POINT ( 'NONE',  ( -2.096375399687082197, 190.2200455327031534, 274.6112675210154634 ) ) ;
#13643 = ORIENTED_EDGE ( 'NONE', *, *, #11970, .T. ) ;
#13644 = CIRCLE ( 'NONE', #2629, 1.999999999999998002 ) ;
#13645 = ADVANCED_FACE ( 'NONE', ( #2798 ), #13352, .T. ) ;
#13646 = CIRCLE ( 'NONE', #13274, 2.000000000000005329 ) ;
#13647 = PLANE ( 'NONE',  #14412 ) ;
#13648 = AXIS2_PLACEMENT_3D ( 'NONE', #3177, #15392, #13877 ) ;
#13649 = DIRECTION ( 'NONE',  ( -0.9999164797902015955, -6.965998958219364448E-18, 0.01292414190464157182 ) ) ;
#13650 = CARTESIAN_POINT ( 'NONE',  ( 17.63467579678667008, 146.7507910439422858, 277.9425923883162568 ) ) ;
#13651 = ORIENTED_EDGE ( 'NONE', *, *, #2069, .F. ) ;
#13652 = CARTESIAN_POINT ( 'NONE',  ( 12.84540398394166871, 188.0649948051286344, 320.9599377868520378 ) ) ;
#13653 = CIRCLE ( 'NONE', #12556, 8.000000000000007105 ) ;
#13654 = MECHANICAL_DESIGN_GEOMETRIC_PRESENTATION_REPRESENTATION (  '', ( #9989 ), #16982 ) ;
#13655 = DIRECTION ( 'NONE',  ( -7.125109674403838460E-05, 0.9999848031710254492, -0.005512562950847868688 ) ) ;
#13656 = EDGE_CURVE ( 'NONE', #1745, #22420, #13204, .T. ) ;
#13657 = DIRECTION ( 'NONE',  ( 2.025474946048326158E-22, -1.000000000000000000, 1.876735158486679638E-22 ) ) ;
#13658 = EDGE_CURVE ( 'NONE', #7377, #9416, #2707, .T. ) ;
#13659 = DIRECTION ( 'NONE',  ( 0.9999164797902015955, 6.965998958219364448E-18, -0.01292414190464157182 ) ) ;
#13660 = CIRCLE ( 'NONE', #13290, 14.36898871458908111 ) ;
#13661 = ORIENTED_EDGE ( 'NONE', *, *, #17372, .T. ) ;
#13662 = CARTESIAN_POINT ( 'NONE',  ( -61.67516800463454985, 127.4153035195788561, 257.6560318593087686 ) ) ;
#13663 = ORIENTED_EDGE ( 'NONE', *, *, #5816, .F. ) ;
#13664 = CARTESIAN_POINT ( 'NONE',  ( 4.195452682864946325, 166.7895964344300808, 324.5942600080963985 ) ) ;
#13665 = CIRCLE ( 'NONE', #16622, 1.999999999999999112 ) ;
#13666 = LINE ( 'NONE', #17454, #4068 ) ;
#13667 = APPLICATION_CONTEXT ( 'automotive_design' ) ;
#13668 = DIRECTION ( 'NONE',  ( -0.1136178953597573593, 0.9935164314186355483, -0.004009283626633517415 ) ) ;
#13669 = CARTESIAN_POINT ( 'NONE',  ( -56.88982296092818558, 126.2575686056375304, 47.57983110662539161 ) ) ;
#13670 = VECTOR ( 'NONE', #9365, 1000.000000000000227 ) ;
#13671 = DIRECTION ( 'NONE',  ( 0.01292394549866733230, 0.005513023399720419666, 0.9999012842304692006 ) ) ;
#13672 = AXIS2_PLACEMENT_3D ( 'NONE', #17569, #12510, #19498 ) ;
#13673 = AXIS2_PLACEMENT_3D ( 'NONE', #21422, #14564, #7633 ) ;
#13674 = CARTESIAN_POINT ( 'NONE',  ( -45.80028074091057988, 166.4461343731306613, 244.9249310372943285 ) ) ;
#13675 = APPLICATION_PROTOCOL_DEFINITION ( 'draft international standard', 'automotive_design', 1998, #3084 ) ;
#13677 = ORIENTED_EDGE ( 'NONE', *, *, #8066, .T. ) ;
#13676 = VERTEX_POINT ( 'NONE', #6033 ) ;
#13678 = DIRECTION ( 'NONE',  ( -0.9999164797902015955, -6.965998958219364448E-18, 0.01292414190464157182 ) ) ;
#13679 = DIRECTION ( 'NONE',  ( -0.000000000000000000, -1.000000000000000000, 0.000000000000000000 ) ) ;
#13680 = FACE_OUTER_BOUND ( 'NONE', #22074, .T. ) ;
#13681 = VECTOR ( 'NONE', #8270, 1000.000000000000114 ) ;
#13682 = DIRECTION ( 'NONE',  ( 7.125109674160258889E-05, -0.9999848031710252272, 0.005512562950849897447 ) ) ;
#13683 = CARTESIAN_POINT ( 'NONE',  ( -90.00000000000000000, 29.00000000000000355, 8.394090934816448357E-16 ) ) ;
#13684 = CARTESIAN_POINT ( 'NONE',  ( -41.99321460073838352, 124.0006990541328804, 0.7963918557340313731 ) ) ;
#13685 = EDGE_CURVE ( 'NONE', #10904, #9306, #4550, .T. ) ;
#13686 = EDGE_LOOP ( 'NONE', ( #10209, #8702, #2830, #17289 ) ) ;
#13687 = CARTESIAN_POINT ( 'NONE',  ( 51.31288912873903740, 109.9913629100859254, -44.83676205748413679 ) ) ;
#13688 = ORIENTED_EDGE ( 'NONE', *, *, #6726, .F. ) ;
#13689 =( BOUNDED_SURFACE ( )  B_SPLINE_SURFACE ( 3, 2, ( 
 ( #14319, #12468, #400 ),
 ( #3501, #2014, #9111 ),
 ( #17528, #8758, #12704 ),
 ( #10859, #9003, #9232 ),
 ( #17884, #19671, #19571 ),
 ( #10962, #3605, #16279 ),
 ( #3941, #19456, #7396 ),
 ( #8889, #16160, #17988 ),
 ( #7519, #5435, #10516 ),
 ( #14547, #15935, #19346 ),
 ( #1781, #7059, #284 ),
 ( #14090, #182, #21073 ),
 ( #7177, #21286, #14207 ),
 ( #5326, #12365, #21181 ),
 ( #3722, #10742, #16049 ),
 ( #19903, #18106, #7620 ),
 ( #18546, #14662, #16493 ),
 ( #20119, #9456, #15111 ) ),
 .UNSPECIFIED., .F., .F., .T. ) 
 B_SPLINE_SURFACE_WITH_KNOTS ( ( 4, 2, 2, 2, 2, 2, 2, 2, 4 ),
 ( 3, 3 ),
 ( 0.003005090483489993892, 0.003807341501471060968, 0.004609592519452128043, 0.005411843537433195551, 0.006214094555414263060, 0.007016345573395330569, 0.007818596591376398078, 0.008620847609357464719, 0.009423098627338533095 ),
 ( 0.000000000000000000, 1.000000000000000000 ),
 .UNSPECIFIED. ) 
 GEOMETRIC_REPRESENTATION_ITEM ( )  RATIONAL_B_SPLINE_SURFACE ( (
 ( 1.000000000000000000, 0.7071067811865479058, 1.000000000000000000),
 ( 1.000000000000000000, 0.6996407321458223416, 1.000000000000000000),
 ( 1.000000000000000000, 0.6923367522679467756, 1.000000000000000000),
 ( 1.000000000000000000, 0.6780525511370015801, 1.000000000000000000),
 ( 1.000000000000000000, 0.6710180578253038819, 1.000000000000000000),
 ( 1.000000000000000000, 0.6575437683264738764, 1.000000000000000000),
 ( 1.000000000000000000, 0.6511910073848069525, 1.000000000000000000),
 ( 1.000000000000000000, 0.6392329869082525873, 1.000000000000000000),
 ( 1.000000000000000000, 0.6335699185534187095, 1.000000000000000000),
 ( 1.000000000000000000, 0.6233860397583550483, 1.000000000000000000),
 ( 1.000000000000000000, 0.6188536248677808382, 1.000000000000000000),
 ( 1.000000000000000000, 0.6108845495338327547, 1.000000000000000000),
 ( 1.000000000000000000, 0.6074396204518591746, 1.000000000000000000),
 ( 1.000000000000000000, 0.6019717515917274442, 1.000000000000000000),
 ( 1.000000000000000000, 0.5998961748957651885, 1.000000000000000000),
 ( 1.000000000000000000, 0.5970819659647461641, 1.000000000000000000),
 ( 1.000000000000000000, 0.5963755918898637765, 1.000000000000000000),
 ( 1.000000000000000000, 0.5963808372950819559, 1.000000000000000000) ) ) 
 REPRESENTATION_ITEM ( '' )  SURFACE ( )  );
#13690 = DIRECTION ( 'NONE',  ( 0.01111468050521610164, -0.5103046645782707280, 0.8599218645824314722 ) ) ;
#13691 = LINE ( 'NONE', #20673, #20075 ) ;
#13692 = B_SPLINE_CURVE_WITH_KNOTS ( 'NONE', 3,
 ( #3939, #9454, #7740, #21504, #10960, #14779, #17986, #21730, #517, #18104, #7517, #5770, #2347, #1535, #22288, #21945, #6242, #17270, #15232, #13388 ),
 .UNSPECIFIED., .F., .F.,
 ( 4, 2, 2, 2, 2, 2, 2, 2, 2, 4 ),
 ( 0.000000000000000000, 0.001733977894910813684, 0.003467955789821627367, 0.005201933684732441485, 0.006935911579643254735, 0.01040386736946483266, 0.01213784526437566152, 0.01300483421183110805, 0.01343832868555880182, 0.01387182315928649386 ),
 .UNSPECIFIED. ) ;
#13693 = LINE ( 'NONE', #22039, #9544 ) ;
#13694 = CIRCLE ( 'NONE', #18458, 7.499999999999991118 ) ;
#13695 = AXIS2_PLACEMENT_3D ( 'NONE', #8046, #1055, #1180 ) ;
#13696 = DIRECTION ( 'NONE',  ( -0.9999164797902017066, -2.045740421681430110E-15, 0.01292414190464156835 ) ) ;
#13697 = CARTESIAN_POINT ( 'NONE',  ( -164.0000000000000000, 20.00000000000000000, 10.00000000000001954 ) ) ;
#13698 = ORIENTED_EDGE ( 'NONE', *, *, #1645, .T. ) ;
#13699 = DIRECTION ( 'NONE',  ( -0.01292414190464044946, -1.902755938799528593E-22, -0.9999164797902015955 ) ) ;
#13700 = ORIENTED_EDGE ( 'NONE', *, *, #14897, .F. ) ;
#13701 = CARTESIAN_POINT ( 'NONE',  ( -65.88241411543796744, 104.3814432989690602, -67.85066342192638444 ) ) ;
#13702 = EDGE_CURVE ( 'NONE', #6945, #10824, #11432, .T. ) ;
#13703 = CARTESIAN_POINT ( 'NONE',  ( -90.15184476568182959, 87.27496089121102329, 51.23113957728794077 ) ) ;
#13704 = AXIS2_PLACEMENT_3D ( 'NONE', #15472, #6823, #11668 ) ;
#13705 = VERTEX_POINT ( 'NONE', #8685 ) ;
#13706 = AXIS2_PLACEMENT_3D ( 'NONE', #20219, #4486, #11516 ) ;
#13707 = DIRECTION ( 'NONE',  ( 7.125109674403838460E-05, -0.9999848031710254492, 0.005512562950847868688 ) ) ;
#13708 = DIRECTION ( 'NONE',  ( -0.9999164797902015955, -6.965998958219364448E-18, 0.01292414190464157182 ) ) ;
#13709 = FACE_OUTER_BOUND ( 'NONE', #7486, .T. ) ;
#13710 = SURFACE_STYLE_FILL_AREA ( #22607 ) ;
#13711 = CARTESIAN_POINT ( 'NONE',  ( -89.24601225622836864, 80.14389198580502693, -29.68648583522428908 ) ) ;
#13712 = DIRECTION ( 'NONE',  ( -5.440186201345785633E-18, -1.000000000000000000, -1.334940939666367878E-17 ) ) ;
#13713 = VERTEX_POINT ( 'NONE', #12167 ) ;
#13714 = VERTEX_POINT ( 'NONE', #12047 ) ;
#13715 = ORIENTED_EDGE ( 'NONE', *, *, #11840, .T. ) ;
#13716 = DIRECTION ( 'NONE',  ( 0.9999164797902017066, 2.001050586450178931E-22, -0.01292414190464131508 ) ) ;
#13717 = CARTESIAN_POINT ( 'NONE',  ( -2.503839020269049254, 159.3664414540641587, 324.7217779040802270 ) ) ;
#13718 = CIRCLE ( 'NONE', #3795, 2.000000000000004885 ) ;
#13719 = CARTESIAN_POINT ( 'NONE',  ( 28.96536656690224021, 99.74539563421257071, 74.50764472524521409 ) ) ;
#13720 = DIRECTION ( 'NONE',  ( 0.9999164797902014845, 0.000000000000000000, -0.01292414190465219874 ) ) ;
#13721 = EDGE_CURVE ( 'NONE', #16143, #10785, #1379, .T. ) ;
#13722 = EDGE_CURVE ( 'NONE', #15636, #2773, #12644, .T. ) ;
#13723 = CARTESIAN_POINT ( 'NONE',  ( -9.411766176742821344, 145.1181305486205702, 276.4045370640140504 ) ) ;
#13724 = SURFACE_SIDE_STYLE ('',( #12106 ) ) ;
#13725 = VECTOR ( 'NONE', #14891, 1000.000000000000227 ) ;
#13726 = CIRCLE ( 'NONE', #11146, 11.00000000000000178 ) ;
#13727 = CARTESIAN_POINT ( 'NONE',  ( -9.829296516163982034, 187.6860858752735908, 321.1599732488574546 ) ) ;
#13728 = VERTEX_POINT ( 'NONE', #19381 ) ;
#13729 = ORIENTED_EDGE ( 'NONE', *, *, #17520, .F. ) ;
#13730 = ORIENTED_EDGE ( 'NONE', *, *, #19183, .T. ) ;
#13731 = EDGE_CURVE ( 'NONE', #3377, #16056, #11543, .T. ) ;
#13732 = CARTESIAN_POINT ( 'NONE',  ( -24.71812196488931690, 189.4003865961453528, -108.5061595206230720 ) ) ;
#13733 = VECTOR ( 'NONE', #6550, 999.9999999999998863 ) ;
#13734 = ORIENTED_EDGE ( 'NONE', *, *, #13036, .F. ) ;
#13735 = EDGE_CURVE ( 'NONE', #6286, #14017, #3427, .T. ) ;
#13736 = DIRECTION ( 'NONE',  ( 1.000000000000000000, 0.000000000000000000, 1.362186893977296347E-14 ) ) ;
#13737 = DIRECTION ( 'NONE',  ( -2.025474946048326158E-22, 1.000000000000000000, -1.876735158486679638E-22 ) ) ;
#13738 = AXIS2_PLACEMENT_3D ( 'NONE', #19020, #1044, #16903 ) ;
#13739 = VECTOR ( 'NONE', #10474, 1000.000000000000114 ) ;
#13740 = CARTESIAN_POINT ( 'NONE',  ( 85.44631271373334869, 75.05144267248711287, 2.026989630736137471 ) ) ;
#13741 = CARTESIAN_POINT ( 'NONE',  ( -93.58499681124557412, 69.99999999999998579, -57.80872228166919058 ) ) ;
#13742 = CARTESIAN_POINT ( 'NONE',  ( -55.33894950108811628, 126.9191314136040063, 167.5679852142817197 ) ) ;
#13743 = CARTESIAN_POINT ( 'NONE',  ( 9.142505149400571796, 81.19615242270661781, -88.65345271381767134 ) ) ;
#13744 = CARTESIAN_POINT ( 'NONE',  ( 3.316624388958365088, 166.4147108432491109, 256.6009726804241495 ) ) ;
#13745 = CARTESIAN_POINT ( 'NONE',  ( -16.53223089048701056, 175.6255473142593644, 113.6748494209804363 ) ) ;
#13746 = CARTESIAN_POINT ( 'NONE',  ( -52.03388546434464246, 189.5999951618935597, -71.94389034825996987 ) ) ;
#13747 = EDGE_CURVE ( 'NONE', #3481, #11404, #521, .T. ) ;
#13748 = FACE_OUTER_BOUND ( 'NONE', #20393, .T. ) ;
#13749 = ORIENTED_EDGE ( 'NONE', *, *, #12469, .F. ) ;
#13750 = AXIS2_PLACEMENT_3D ( 'NONE', #16667, #8254, #8140 ) ;
#13751 = FACE_BOUND ( 'NONE', #8558, .T. ) ;
#13752 = CARTESIAN_POINT ( 'NONE',  ( -9.979532414892725356, 187.9007632834477306, 308.1559136815830016 ) ) ;
#13753 = ORIENTED_EDGE ( 'NONE', *, *, #6069, .F. ) ;
#13754 = VECTOR ( 'NONE', #12961, 1000.000000000000227 ) ;
#13755 = VERTEX_POINT ( 'NONE', #20761 ) ;
#13756 = VECTOR ( 'NONE', #19661, 1000.000000000000227 ) ;
#13757 = CARTESIAN_POINT ( 'NONE',  ( -2.322807172541347498, 69.99999999999998579, -81.06750429846923112 ) ) ;
#13758 = ADVANCED_FACE ( 'NONE', ( #19270 ), #10326, .F. ) ;
#13759 = AXIS2_PLACEMENT_3D ( 'NONE', #3586, #15676, #22619 ) ;
#13760 = ORIENTED_EDGE ( 'NONE', *, *, #9779, .T. ) ;
#13761 = DIRECTION ( 'NONE',  ( 0.9999164797902017066, 2.001050586450178931E-22, -0.01292414190464131508 ) ) ;
#13762 = CARTESIAN_POINT ( 'NONE',  ( 17.14453832658934829, 137.4882992087673870, 88.44737388259316901 ) ) ;
#13763 = FACE_OUTER_BOUND ( 'NONE', #21091, .T. ) ;
#13764 = VERTEX_POINT ( 'NONE', #13975 ) ;
#13765 = CARTESIAN_POINT ( 'NONE',  ( 13.32375866196222347, 190.1420591301118748, 320.8223493350537865 ) ) ;
#13766 = EDGE_CURVE ( 'NONE', #20506, #12670, #14493, .T. ) ;
#13767 = CARTESIAN_POINT ( 'NONE',  ( 109.9311545250608617, 74.99990065235996894, -6.043940776851986385 ) ) ;
#13768 = DIRECTION ( 'NONE',  ( -0.008930640170465353744, -0.5047668041246317072, -0.8632095441548079950 ) ) ;
#13769 = DIRECTION ( 'NONE',  ( 0.3101392564284313202, 0.9506461370142480494, -0.009250070373107143265 ) ) ;
#13770 = ORIENTED_EDGE ( 'NONE', *, *, #18976, .T. ) ;
#13771 = DIRECTION ( 'NONE',  ( 0.6295830517327242193, 0.6486237524303245516, 0.4276826028190943152 ) ) ;
#13772 = VERTEX_POINT ( 'NONE', #21108 ) ;
#13773 = DIRECTION ( 'NONE',  ( -0.01292394549866727679, -0.005513023399720743192, -0.9999012842304693116 ) ) ;
#13774 = DIRECTION ( 'NONE',  ( 0.000000000000000000, -1.000000000000000000, 0.000000000000000000 ) ) ;
#13775 = CARTESIAN_POINT ( 'NONE',  ( 1.117803423002105445, 55.00000000000000000, 109.6947150755565161 ) ) ;
#13776 = CARTESIAN_POINT ( 'NONE',  ( 44.31784132852413194, 168.2105890667581605, -53.06813496338226344 ) ) ;
#13777 = DIRECTION ( 'NONE',  ( 0.8981428216242087759, 0.000000000000000000, 0.4397038457472314255 ) ) ;
#13778 = DIRECTION ( 'NONE',  ( -0.01220060921879500236, -0.3298969072164960603, -0.9439381207174974975 ) ) ;
#13779 = LINE ( 'NONE', #12049, #11710 ) ;
#13780 = DIRECTION ( 'NONE',  ( -0.01292414190463830014, 0.000000000000000000, -0.9999164797902017066 ) ) ;
#13781 = EDGE_CURVE ( 'NONE', #20909, #5578, #11576, .T. ) ;
#13782 = EDGE_CURVE ( 'NONE', #12812, #11335, #19942, .T. ) ;
#13783 = ORIENTED_EDGE ( 'NONE', *, *, #20623, .F. ) ;
#13784 = CARTESIAN_POINT ( 'NONE',  ( -36.93353118839863924, 92.00280690333769940, 84.44237658584599160 ) ) ;
#13785 = CARTESIAN_POINT ( 'NONE',  ( -48.67164386273223187, 109.5652376256254854, -43.54209035921780213 ) ) ;
#13786 = CARTESIAN_POINT ( 'NONE',  ( -65.59152507611121052, 113.4706157781613598, -45.34512716587771308 ) ) ;
#13787 = CARTESIAN_POINT ( 'NONE',  ( -93.21002351426726307, 69.99999999999998579, -28.79774562292281104 ) ) ;
#13788 = CARTESIAN_POINT ( 'NONE',  ( -4.505147608247620283, 176.8666157021447134, 324.6511568656583222 ) ) ;
#13789 = VECTOR ( 'NONE', #7805, 1000.000000000000227 ) ;
#13790 = ORIENTED_EDGE ( 'NONE', *, *, #8058, .F. ) ;
#13791 = DIRECTION ( 'NONE',  ( 0.9934404589540163366, 0.1135548637187043797, -0.01346653032742958257 ) ) ;
#13792 = PRODUCT_DEFINITION_SHAPE ( 'NONE', 'NONE',  #22692 ) ;
#13793 = CARTESIAN_POINT ( 'NONE',  ( -19.00623411919002592, 140.4227465520235967, 77.01503843080352851 ) ) ;
#13794 = ORIENTED_EDGE ( 'NONE', *, *, #16537, .T. ) ;
#13795 = CARTESIAN_POINT ( 'NONE',  ( 47.76182451837959064, 110.4323045661290337, -44.79329492277620517 ) ) ;
#13796 = ORIENTED_EDGE ( 'NONE', *, *, #4916, .T. ) ;
#13797 = CARTESIAN_POINT ( 'NONE',  ( 41.22194066120597000, 125.3750519639578727, 249.0299023193002768 ) ) ;
#13798 = CARTESIAN_POINT ( 'NONE',  ( -8.580473483290074199, 70.00000000000001421, -95.10893838946512346 ) ) ;
#13799 = DIRECTION ( 'NONE',  ( -0.01292394549866632963, -0.005513023399716958026, -0.9999012842304692006 ) ) ;
#13800 = CARTESIAN_POINT ( 'NONE',  ( -53.12424548001075664, 118.8900173874207837, 162.2800983528087215 ) ) ;
#13801 = ORIENTED_EDGE ( 'NONE', *, *, #20006, .T. ) ;
#13802 = DIRECTION ( 'NONE',  ( -0.9934404589540162256, -0.1135548637187056842, 0.01346653032743081423 ) ) ;
#13803 = CARTESIAN_POINT ( 'NONE',  ( -55.33894950108835076, 126.9191314136037789, 167.5679852142818334 ) ) ;
#13804 = ORIENTED_EDGE ( 'NONE', *, *, #12095, .T. ) ;
#13805 = CARTESIAN_POINT ( 'NONE',  ( 49.23668000689734470, 95.70300605291201634, -45.90578145146270117 ) ) ;
#13806 = FACE_OUTER_BOUND ( 'NONE', #14341, .T. ) ;
#13807 = ORIENTED_EDGE ( 'NONE', *, *, #14353, .T. ) ;
#13808 = CARTESIAN_POINT ( 'NONE',  ( 92.05960170301050027, 69.99999999999998579, -60.20821982323567312 ) ) ;
#13809 = CARTESIAN_POINT ( 'NONE',  ( -90.09760470754743267, 87.49028989906726395, 51.09979543946362668 ) ) ;
#13810 = B_SPLINE_CURVE_WITH_KNOTS ( 'NONE', 3,
 ( #2541, #6094, #16461, #7931, #4134, #19746, #10930, #708, #13120, #4355 ),
 .UNSPECIFIED., .F., .F.,
 ( 4, 2, 2, 2, 4 ),
 ( 0.000000000000000000, 0.0004370559136044528279, 0.0008741118272089056559, 0.001311167740813358375, 0.001748223654417811312 ),
 .UNSPECIFIED. ) ;
#13811 = DIRECTION ( 'NONE',  ( 0.1136178953597579561, -0.9935164314186356593, 0.004009283626633661397 ) ) ;
#13813 = EDGE_LOOP ( 'NONE', ( #14537, #6693, #4633, #11977 ) ) ;
#13812 = ORIENTED_EDGE ( 'NONE', *, *, #6514, .F. ) ;
#13814 = EDGE_LOOP ( 'NONE', ( #2032, #7822, #5738, #611 ) ) ;
#13815 = CARTESIAN_POINT ( 'NONE',  ( -56.92213282467484703, 126.2437860471382294, 45.08007789604923232 ) ) ;
#13816 =( BOUNDED_SURFACE ( )  B_SPLINE_SURFACE ( 3, 2, ( 
 ( #8934, #218, #7215 ),
 ( #19156, #19500, #14243 ),
 ( #21218, #5476, #17462 ),
 ( #11634, #2561, #2889 ) ),
 .UNSPECIFIED., .F., .F., .T. ) 
 B_SPLINE_SURFACE_WITH_KNOTS ( ( 4, 4 ),
 ( 3, 3 ),
 ( 0.4226013619543070310, 0.4841788640348457240 ),
 ( 0.000000000000000000, 1.000000000000000000 ),
 .UNSPECIFIED. ) 
 GEOMETRIC_REPRESENTATION_ITEM ( )  RATIONAL_B_SPLINE_SURFACE ( (
 ( 1.000000000000000000, 0.9068900557993654354, 1.000000000000000000),
 ( 1.000000000000000000, 0.9052491015987689238, 1.000000000000000000),
 ( 1.000000000000000000, 0.9034913259101540195, 1.000000000000000000),
 ( 1.000000000000000000, 0.9016180287879275168, 1.000000000000000000) ) ) 
 REPRESENTATION_ITEM ( '' )  SURFACE ( )  );
#13817 = CARTESIAN_POINT ( 'NONE',  ( -92.43457499998879712, 72.00000000000000000, 31.19724316448926160 ) ) ;
#13818 = CARTESIAN_POINT ( 'NONE',  ( -51.36859115140752152, 114.2028473779704143, 164.5977368973751993 ) ) ;
#13819 = CARTESIAN_POINT ( 'NONE',  ( -10.85980368455889433, 163.6991139211620236, 126.9796742121690443 ) ) ;
#13820 = DIRECTION ( 'NONE',  ( -0.01292394549866740690, -0.005513023399721241925, -0.9999012842304693116 ) ) ;
#13821 = CARTESIAN_POINT ( 'NONE',  ( -44.25520882077128704, 168.2183454221810734, 273.2074843050344271 ) ) ;
#13822 = ORIENTED_EDGE ( 'NONE', *, *, #11348, .T. ) ;
#13823 = VERTEX_POINT ( 'NONE', #16070 ) ;
#13824 = CARTESIAN_POINT ( 'NONE',  ( -8.560375375394391639, 187.5535857524832295, 277.4257007466420646 ) ) ;
#13825 = LINE ( 'NONE', #16022, #20678 ) ;
#13826 = LINE ( 'NONE', #11880, #10535 ) ;
#13827 = CARTESIAN_POINT ( 'NONE',  ( -1.163172771417702700, 81.99999999999998579, -89.99248318111824574 ) ) ;
#13828 = CARTESIAN_POINT ( 'NONE',  ( -1.632550740186646143, 142.7036636415817838, 274.8672572718561469 ) ) ;
#13829 = ORIENTED_EDGE ( 'NONE', *, *, #22130, .T. ) ;
#13830 = DIRECTION ( 'NONE',  ( 1.000000000000000000, 0.000000000000000000, 0.000000000000000000 ) ) ;
#13831 = CARTESIAN_POINT ( 'NONE',  ( -7.337194850064199692, 109.6999844229167564, 127.2409188565385421 ) ) ;
#13832 = DIRECTION ( 'NONE',  ( -0.01292394549866740169, -0.005513023399721021615, -0.9999012842304692006 ) ) ;
#13833 =( REPRESENTATION_RELATIONSHIP ('NONE','NONE', #11808, #3137 ) REPRESENTATION_RELATIONSHIP_WITH_TRANSFORMATION ( #107 )SHAPE_REPRESENTATION_RELATIONSHIP( ) );
#13834 = CARTESIAN_POINT ( 'NONE',  ( -64.01537291612297054, 100.1864212328113979, 76.59879228792688366 ) ) ;
#13835 = ORIENTED_EDGE ( 'NONE', *, *, #12969, .F. ) ;
#13836 = ORIENTED_EDGE ( 'NONE', *, *, #16525, .T. ) ;
#13837 = UNCERTAINTY_MEASURE_WITH_UNIT (LENGTH_MEASURE( 1.000000000000000082E-05 ), #17274, 'distance_accuracy_value', 'NONE');
#13838 = DIRECTION ( 'NONE',  ( 0.9999164797902015955, 6.965998958219364448E-18, -0.01292414190464157182 ) ) ;
#13839 = EDGE_CURVE ( 'NONE', #13165, #20787, #10415, .T. ) ;
#13840 = EDGE_LOOP ( 'NONE', ( #2106, #11107, #6153, #15418 ) ) ;
#13841 = DIRECTION ( 'NONE',  ( 0.000000000000000000, 0.000000000000000000, -1.000000000000000000 ) ) ;
#13842 = DIRECTION ( 'NONE',  ( 0.9999164797902015955, 2.001050586498092550E-22, -0.01292414190464117457 ) ) ;
#13843 = FACE_OUTER_BOUND ( 'NONE', #14395, .T. ) ;
#13844 = CARTESIAN_POINT ( 'NONE',  ( -91.81287659828484493, 71.13119029400843374, -60.58394261007859427 ) ) ;
#13845 = CARTESIAN_POINT ( 'NONE',  ( 43.19632491693555210, 119.7615706795621691, 247.0351358235509167 ) ) ;
#13846 = DIRECTION ( 'NONE',  ( -7.125109674118361251E-05, 0.9999848031710253382, -0.005512562950849477644 ) ) ;
#13847 = CARTESIAN_POINT ( 'NONE',  ( -52.93127853433226448, 189.6011917897851333, -71.71522176735570042 ) ) ;
#13848 = DIRECTION ( 'NONE',  ( -2.025474946048326158E-22, 1.000000000000000000, -1.876735158486678933E-22 ) ) ;
#13849 = EDGE_CURVE ( 'NONE', #5713, #12267, #8911, .T. ) ;
#13850 = CYLINDRICAL_SURFACE ( 'NONE', #9565, 85.00000000000001421 ) ;
#13851 = ORIENTED_EDGE ( 'NONE', *, *, #15823, .T. ) ;
#13852 = AXIS2_PLACEMENT_3D ( 'NONE', #9853, #8009, #13955 ) ;
#13853 = EDGE_CURVE ( 'NONE', #6959, #9437, #17414, .T. ) ;
#13854 = DIRECTION ( 'NONE',  ( -0.01292394549866731669, -0.005513023399720593139, -0.9999012842304692006 ) ) ;
#13855 = FACE_OUTER_BOUND ( 'NONE', #4535, .T. ) ;
#13856 = ORIENTED_EDGE ( 'NONE', *, *, #16190, .F. ) ;
#13857 = CARTESIAN_POINT ( 'NONE',  ( -1.432836755002403442E-14, 25.00000000000000000, -117.0000000000000000 ) ) ;
#13858 = ORIENTED_EDGE ( 'NONE', *, *, #3321, .F. ) ;
#13859 = EDGE_CURVE ( 'NONE', #1058, #12670, #7302, .T. ) ;
#13860 = DIRECTION ( 'NONE',  ( 0.01292394549866738782, 0.005513023399720700692, 0.9999012842304693116 ) ) ;
#13861 = ADVANCED_FACE ( 'NONE', ( #19928 ), #12831, .T. ) ;
#13862 = ADVANCED_FACE ( 'NONE', ( #13157 ), #20120, .T. ) ;
#13863 = CARTESIAN_POINT ( 'NONE',  ( 0.3234033260118191477, 327.3504727214124728, 314.5682625988872587 ) ) ;
#13864 = CIRCLE ( 'NONE', #21543, 5.999999999999999112 ) ;
#13865 = DIRECTION ( 'NONE',  ( 0.009985269297341583389, 0.6348858185549669519, 0.7725414498878678815 ) ) ;
#13866 = ORIENTED_EDGE ( 'NONE', *, *, #18951, .T. ) ;
#13867 = DIRECTION ( 'NONE',  ( 0.8981428216242088869, 0.000000000000000000, 0.4397038457472307593 ) ) ;
#13868 = EDGE_LOOP ( 'NONE', ( #324, #12453 ) ) ;
#13869 = CARTESIAN_POINT ( 'NONE',  ( 48.79414080053240355, 189.4876967392748384, -93.61816863908353525 ) ) ;
#13870 = CARTESIAN_POINT ( 'NONE',  ( 107.5937258339208142, 77.46195535017201905, -22.91004653791229018 ) ) ;
#13871 = ORIENTED_EDGE ( 'NONE', *, *, #13281, .T. ) ;
#13872 = CARTESIAN_POINT ( 'NONE',  ( 107.9412751340845489, 77.72595396897827413, 21.65777188997737213 ) ) ;
#13873 = DIRECTION ( 'NONE',  ( -0.007270543169446415203, -0.7109943187548720678, -0.7031601651830943212 ) ) ;
#13874 = ADVANCED_FACE ( 'NONE', ( #17548 ), #7476, .T. ) ;
#13875 = ORIENTED_EDGE ( 'NONE', *, *, #16263, .T. ) ;
#13876 = VECTOR ( 'NONE', #3161, 1000.000000000000227 ) ;
#13877 = DIRECTION ( 'NONE',  ( 0.6916826046072646061, 0.7220860138273254014, -0.01292142092318427499 ) ) ;
#13878 = EDGE_CURVE ( 'NONE', #13100, #650, #2735, .T. ) ;
#13879 = DIRECTION ( 'NONE',  ( 0.000000000000000000, 1.000000000000000000, -0.000000000000000000 ) ) ;
#13880 = CARTESIAN_POINT ( 'NONE',  ( -79.90518398323658289, 100.1635695855007668, -75.81005614957796013 ) ) ;
#13881 = DIRECTION ( 'NONE',  ( 0.9999164797902015955, 6.965998958219364448E-18, -0.01292414190464157182 ) ) ;
#13882 = AXIS2_PLACEMENT_3D ( 'NONE', #688, #9167, #2293 ) ;
#13883 = CARTESIAN_POINT ( 'NONE',  ( 55.40268456415108744, 18.00000000000000355, 113.1659955246503557 ) ) ;
#13884 = CARTESIAN_POINT ( 'NONE',  ( -58.43812057966402307, 118.9192529882355842, 167.6521505577929645 ) ) ;
#13885 = ORIENTED_EDGE ( 'NONE', *, *, #3172, .F. ) ;
#13886 = DIRECTION ( 'NONE',  ( 0.9999164797902017066, 2.001050586498092786E-22, -0.01292414190464117631 ) ) ;
#13887 = DIRECTION ( 'NONE',  ( 0.01292394549866733230, 0.005513023399720419666, 0.9999012842304692006 ) ) ;
#13888 = EDGE_CURVE ( 'NONE', #2665, #1225, #8222, .T. ) ;
#13889 = VECTOR ( 'NONE', #4401, 1000.000000000000227 ) ;
#13890 = ORIENTED_EDGE ( 'NONE', *, *, #16286, .T. ) ;
#13891 = CYLINDRICAL_SURFACE ( 'NONE', #20620, 10.00000000000000888 ) ;
#13892 = DIRECTION ( 'NONE',  ( 5.440186201345810285E-18, 1.000000000000000000, 1.334940939666369727E-17 ) ) ;
#13893 = SPHERICAL_SURFACE ( 'NONE', #16560, 2.000000000000000000 ) ;
#13894 = DIRECTION ( 'NONE',  ( -0.01292394549866750231, -0.005513023399722823126, -0.9999012842304692006 ) ) ;
#13895 = ORIENTED_EDGE ( 'NONE', *, *, #21417, .F. ) ;
#13896 = DIRECTION ( 'NONE',  ( -0.9934404589540162256, -0.1135548637187056842, 0.01346653032743081423 ) ) ;
#13897 = CARTESIAN_POINT ( 'NONE',  ( -51.97046013708073531, 113.4377915441418452, -43.52080401654976072 ) ) ;
#13898 = ORIENTED_EDGE ( 'NONE', *, *, #12847, .T. ) ;
#13899 = CARTESIAN_POINT ( 'NONE',  ( 50.82209241344880724, 113.4364193371377638, -44.84941295302596131 ) ) ;
#13900 = ORIENTED_EDGE ( 'NONE', *, *, #9966, .F. ) ;
#13901 = CARTESIAN_POINT ( 'NONE',  ( -89.66113247980429435, 100.6041916471018709, -63.72504470331098503 ) ) ;
#13902 = DIRECTION ( 'NONE',  ( -0.9999164797902017066, -2.001050586450180576E-22, 0.01292414190464044946 ) ) ;
#13903 = DIRECTION ( 'NONE',  ( -0.9999164797902017066, 0.000000000000000000, 0.01292414190463972781 ) ) ;
#13904 = VERTEX_POINT ( 'NONE', #12747 ) ;
#13905 = ADVANCED_FACE ( 'NONE', ( #11135 ), #20175, .F. ) ;
#13906 = DIRECTION ( 'NONE',  ( 0.000000000000000000, 1.000000000000000000, -0.000000000000000000 ) ) ;
#13907 = DIRECTION ( 'NONE',  ( -0.01292394549866731669, -0.005513023399719711899, -0.9999012842304692006 ) ) ;
#13908 = ADVANCED_FACE ( 'NONE', ( #3345 ), #12207, .F. ) ;
#13909 = ORIENTED_EDGE ( 'NONE', *, *, #11346, .T. ) ;
#13910 = CARTESIAN_POINT ( 'NONE',  ( 21.64049994983132663, 168.7353503906255412, 312.3898283681904786 ) ) ;
#13911 = CARTESIAN_POINT ( 'NONE',  ( 9.858392366551100849, 190.0737637416658288, 274.6814703483424864 ) ) ;
#13912 = VECTOR ( 'NONE', #14844, 1000.000000000000114 ) ;
#13913 = VERTEX_POINT ( 'NONE', #20908 ) ;
#13914 = CARTESIAN_POINT ( 'NONE',  ( -66.19625437534079992, 189.4876967392748384, -92.13189232004975793 ) ) ;
#13915 = CARTESIAN_POINT ( 'NONE',  ( -88.16898101804537191, 88.70782710634040313, 52.40912332135838625 ) ) ;
#13916 = CARTESIAN_POINT ( 'NONE',  ( -66.37745437015971106, 69.99999999999997158, -106.1509941137499595 ) ) ;
#13918 = ORIENTED_EDGE ( 'NONE', *, *, #22380, .F. ) ;
#13917 = ORIENTED_EDGE ( 'NONE', *, *, #16711, .F. ) ;
#13919 = ORIENTED_EDGE ( 'NONE', *, *, #8333, .T. ) ;
#13920 = DIRECTION ( 'NONE',  ( 0.4119494117036593406, -0.9111911607883945718, -0.005324537360869059308 ) ) ;
#13921 = CARTESIAN_POINT ( 'NONE',  ( -146.5000000000000000, 18.00000000000000355, -7.999999999999981348 ) ) ;
#13922 = CARTESIAN_POINT ( 'NONE',  ( -16.24193888600903435, 87.34754884532240737, -76.12214651130867082 ) ) ;
#13923 = LINE ( 'NONE', #15330, #16519 ) ;
#13924 = CARTESIAN_POINT ( 'NONE',  ( 83.04991721846113251, 75.08645580250137641, -5.130063099084944511 ) ) ;
#13925 = AXIS2_PLACEMENT_3D ( 'NONE', #15256, #3255, #6720 ) ;
#13926 = LINE ( 'NONE', #10374, #2349 ) ;
#13927 = EDGE_LOOP ( 'NONE', ( #20040, #266, #8504, #14990 ) ) ;
#13928 = ORIENTED_EDGE ( 'NONE', *, *, #15184, .F. ) ;
#13929 = AXIS2_PLACEMENT_3D ( 'NONE', #21674, #5965, #13106 ) ;
#13930 = CARTESIAN_POINT ( 'NONE',  ( -42.64951291394369548, 126.1473081376431367, 27.39440536439884255 ) ) ;
#13931 = LINE ( 'NONE', #19547, #10789 ) ;
#13932 = CARTESIAN_POINT ( 'NONE',  ( -79.59455004317675275, 75.13699351169599083, 6.129203171928941707 ) ) ;
#13933 = CARTESIAN_POINT ( 'NONE',  ( -12.09763426542455811, 164.9045537938005452, 319.1981365539348872 ) ) ;
#13934 = CARTESIAN_POINT ( 'NONE',  ( -105.8287943736951604, 79.03195428549125268, 30.00479353936295368 ) ) ;
#13935 = ORIENTED_EDGE ( 'NONE', *, *, #15574, .F. ) ;
#13936 = EDGE_CURVE ( 'NONE', #5713, #9934, #6894, .T. ) ;
#13937 = CARTESIAN_POINT ( 'NONE',  ( 93.62421092229767794, 69.99999999999998579, 60.84264408248096601 ) ) ;
#13938 = DIRECTION ( 'NONE',  ( 0.000000000000000000, -1.000000000000000000, 0.000000000000000000 ) ) ;
#13939 = CARTESIAN_POINT ( 'NONE',  ( 45.34010913598296355, 168.6466622724117599, 26.02279695137911020 ) ) ;
#13940 = DIRECTION ( 'NONE',  ( -0.000000000000000000, -1.000000000000000000, -0.000000000000000000 ) ) ;
#13941 = EDGE_LOOP ( 'NONE', ( #4493, #19111 ) ) ;
#13942 = CIRCLE ( 'NONE', #16534, 4.374999999999991118 ) ;
#13943 = ORIENTED_EDGE ( 'NONE', *, *, #20534, .F. ) ;
#13944 = COLOUR_RGB ( '', 0.08235294, 0.09019608, 0.10196078) ;
#13945 = CIRCLE ( 'NONE', #5110, 8.520833333333293069 ) ;
#13946 = VERTEX_POINT ( 'NONE', #19189 ) ;
#13947 = PRODUCT_DEFINITION ( 'UNKNOWN', '', #2215, #4889 ) ;
#13948 = VECTOR ( 'NONE', #20294, 1000.000000000000000 ) ;
#13949 = CARTESIAN_POINT ( 'NONE',  ( -65.56790548363530036, 144.7550503794368524, -43.51772385068294113 ) ) ;
#13950 = CARTESIAN_POINT ( 'NONE',  ( 49.99582398951007889, 170.0000000000000284, -0.6462070952321007367 ) ) ;
#13951 = DIRECTION ( 'NONE',  ( -0.01292394549866731843, -0.005513023399720594006, -0.9999012842304693116 ) ) ;
#13952 = CARTESIAN_POINT ( 'NONE',  ( -41.52238611146507452, 166.0448094368137504, 269.1837510020998820 ) ) ;
#13953 = CARTESIAN_POINT ( 'NONE',  ( -90.15896375023012865, 69.98053812266098817, 63.28569483684161412 ) ) ;
#13954 = CARTESIAN_POINT ( 'NONE',  ( -61.67972807482614428, 191.4143309225244707, 257.3032278304543183 ) ) ;
#13955 = DIRECTION ( 'NONE',  ( 0.9909299940865187173, -0.1338359446631179062, -0.01207007604876208194 ) ) ;
#13956 = CARTESIAN_POINT ( 'NONE',  ( -51.42204038937180144, 189.5972346270502271, -72.45256254838918153 ) ) ;
#13957 = AXIS2_PLACEMENT_3D ( 'NONE', #191, #13972, #12377 ) ;
#13958 =( REPRESENTATION_RELATIONSHIP ('NONE','NONE', #11808, #15634 ) REPRESENTATION_RELATIONSHIP_WITH_TRANSFORMATION ( #7320 )SHAPE_REPRESENTATION_RELATIONSHIP( ) );
#13959 = CARTESIAN_POINT ( 'NONE',  ( 89.71476837554287442, 79.66528429935014799, 28.24846625074276929 ) ) ;
#13960 = EDGE_LOOP ( 'NONE', ( #13136, #5194, #11723, #20698 ) ) ;
#13961 = VECTOR ( 'NONE', #4019, 1000.000000000000000 ) ;
#13962 = EDGE_CURVE ( 'NONE', #11132, #4095, #20685, .T. ) ;
#13963 = VECTOR ( 'NONE', #19396, 1000.000000000000114 ) ;
#13964 = CARTESIAN_POINT ( 'NONE',  ( 106.2770331005257276, 184.8436277385793289, -28.37590941890332985 ) ) ;
#13965 = AXIS2_PLACEMENT_3D ( 'NONE', #8119, #19937, #16860 ) ;
#13966 = DIRECTION ( 'NONE',  ( 0.01035335185279115042, 0.005513005182354825326, 0.9999312050732648283 ) ) ;
#13967 = VERTEX_POINT ( 'NONE', #15657 ) ;
#13968 = CARTESIAN_POINT ( 'NONE',  ( -91.13609774473528091, 79.20914543161394761, -26.78943607724156095 ) ) ;
#13969 = ORIENTED_EDGE ( 'NONE', *, *, #22556, .F. ) ;
#13970 = PRODUCT_DEFINITION_SHAPE ( 'NONE', 'NONE',  #22681 ) ;
#13971 = VECTOR ( 'NONE', #3950, 1000.000000000000114 ) ;
#13972 = DIRECTION ( 'NONE',  ( 7.125109674364534776E-05, -0.9999848031710252272, 0.005512562950849704893 ) ) ;
#13973 = EDGE_CURVE ( 'NONE', #7249, #15798, #5051, .T. ) ;
#13974 = VECTOR ( 'NONE', #6986, 1000.000000000000000 ) ;
#13975 = CARTESIAN_POINT ( 'NONE',  ( 80.05923150692980528, 54.99999999999999289, 4.065642694558706971 ) ) ;
#13976 = DIRECTION ( 'NONE',  ( -0.006690748560446689759, 0.8555659502960908380, -0.5176505950712777526 ) ) ;
#13977 = CARTESIAN_POINT ( 'NONE',  ( -9.829281886977605964, 187.6860989516580389, 321.1599752159536365 ) ) ;
#13978 = CARTESIAN_POINT ( 'NONE',  ( 18.54481925875508708, 147.4389108747255364, 278.1650990181268526 ) ) ;
#13979 = ADVANCED_FACE ( 'NONE', ( #15771 ), #3826, .F. ) ;
#13980 = CIRCLE ( 'NONE', #4062, 2.499999999999988010 ) ;
#13981 = ORIENTED_EDGE ( 'NONE', *, *, #18906, .F. ) ;
#13982 = CARTESIAN_POINT ( 'NONE',  ( 12.23383248052724070, 187.6909830581990946, 322.9726054647817364 ) ) ;
#13983 = VERTEX_POINT ( 'NONE', #22601 ) ;
#13984 = CARTESIAN_POINT ( 'NONE',  ( 4.376210989365967308, 69.99999999999998579, -92.29796090835098710 ) ) ;
#13985 = DIRECTION ( 'NONE',  ( 0.01292394549866738261, 0.005513023399722618428, 0.9999012842304692006 ) ) ;
#13986 = DIRECTION ( 'NONE',  ( -0.01292394549866738782, -0.005513023399720468239, -0.9999012842304692006 ) ) ;
#13987 = ORIENTED_EDGE ( 'NONE', *, *, #6118, .F. ) ;
#13988 =( NAMED_UNIT ( * ) SI_UNIT ( $, .STERADIAN. ) SOLID_ANGLE_UNIT ( ) );
#13989 = CARTESIAN_POINT ( 'NONE',  ( -57.55251350461809778, 118.9484885890504557, 172.9440730829682877 ) ) ;
#13990 = EDGE_LOOP ( 'NONE', ( #14549, #6793, #10289, #17977 ) ) ;
#13991 = EDGE_CURVE ( 'NONE', #3529, #11795, #19070, .T. ) ;
#13992 = DIRECTION ( 'NONE',  ( -0.01292394549866632963, -0.005513023399716958026, -0.9999012842304692006 ) ) ;
#13993 = EDGE_CURVE ( 'NONE', #1614, #1930, #16688, .T. ) ;
#13994 = AXIS2_PLACEMENT_3D ( 'NONE', #2810, #9713, #16624 ) ;
#13995 = ADVANCED_FACE ( 'NONE', ( #10788 ), #14132, .F. ) ;
#13996 = ORIENTED_EDGE ( 'NONE', *, *, #16983, .F. ) ;
#13997 = PRODUCT_DEFINITION_SHAPE ( 'NONE', 'NONE',  #9450 ) ;
#13998 = CARTESIAN_POINT ( 'NONE',  ( -90.85853474116407824, 77.59429383720566875, 31.92673238494555221 ) ) ;
#13999 = FACE_OUTER_BOUND ( 'NONE', #22612, .T. ) ;
#14000 = LINE ( 'NONE', #11831, #20184 ) ;
#14001 = CIRCLE ( 'NONE', #19471, 124.0000000000000000 ) ;
#14002 = DIRECTION ( 'NONE',  ( -7.125109674243555432E-05, 0.9999848031710253382, -0.005512562950850175003 ) ) ;
#14003 = VECTOR ( 'NONE', #12731, 1000.000000000000000 ) ;
#14004 = DIRECTION ( 'NONE',  ( 0.7943823600057676737, -1.243025994321580632E-17, 0.6074180324222084870 ) ) ;
#14005 = CARTESIAN_POINT ( 'NONE',  ( 163.9999999999992610, 1.999999999999998224, -53.76161406891485228 ) ) ;
#14006 = DIRECTION ( 'NONE',  ( -0.2311175842251773915, 0.9723818865373500264, 0.03252889478574687993 ) ) ;
#14007 = ADVANCED_FACE ( 'NONE', ( #10444 ), #13816, .T. ) ;
#14008 = CONTEXT_DEPENDENT_SHAPE_REPRESENTATION ( #13833, #4763 ) ;
#14009 = EDGE_CURVE ( 'NONE', #3703, #11287, #10024, .T. ) ;
#14010 = CIRCLE ( 'NONE', #5182, 95.00000000000004263 ) ;
#14011 = CIRCLE ( 'NONE', #50, 2.000000000000004885 ) ;
#14012 = DIRECTION ( 'NONE',  ( 0.01292394549866727679, 0.005513023399720742325, 0.9999012842304692006 ) ) ;
#14013 = EDGE_CURVE ( 'NONE', #1999, #7226, #9693, .T. ) ;
#14014 = FACE_OUTER_BOUND ( 'NONE', #6830, .T. ) ;
#14015 = CARTESIAN_POINT ( 'NONE',  ( 48.31072223536619958, 166.8507685304810764, 256.0170097695137201 ) ) ;
#14016 = DIRECTION ( 'NONE',  ( 0.6933298757296778581, 0.07639711794142929613, -0.7165592535100728799 ) ) ;
#14017 = VERTEX_POINT ( 'NONE', #18629 ) ;
#14018 = VECTOR ( 'NONE', #18064, 999.9999999999998863 ) ;
#14019 = EDGE_LOOP ( 'NONE', ( #16163, #12286 ) ) ;
#14020 = CARTESIAN_POINT ( 'NONE',  ( 17.14453832658934829, 137.4882992087673870, 88.44737388259316901 ) ) ;
#14021 = DIRECTION ( 'NONE',  ( -0.000000000000000000, -1.000000000000000000, 0.000000000000000000 ) ) ;
#14022 = ORIENTED_EDGE ( 'NONE', *, *, #1226, .T. ) ;
#14023 = CARTESIAN_POINT ( 'NONE',  ( 49.79948073228538874, 109.1696245789948847, -44.81267020896142839 ) ) ;
#14024 = CIRCLE ( 'NONE', #4097, 7.499999999999991118 ) ;
#14025 = EDGE_LOOP ( 'NONE', ( #5606, #3926, #21376, #20314, #16319, #13472, #5887, #3260, #12611, #7836 ) ) ;
#14026 =( NAMED_UNIT ( * ) PLANE_ANGLE_UNIT ( ) SI_UNIT ( $, .RADIAN. ) );
#14027 = CARTESIAN_POINT ( 'NONE',  ( -88.72067713466817906, 101.8298110126636260, -65.04826529396217438 ) ) ;
#14028 = DIRECTION ( 'NONE',  ( -0.01292414190529159179, 1.415534356397187034E-10, -0.9999164797901932689 ) ) ;
#14029 = DIRECTION ( 'NONE',  ( -0.01292394549866737914, -0.005513023399721009472, -0.9999012842304692006 ) ) ;
#14030 = EDGE_CURVE ( 'NONE', #14948, #16143, #13375, .T. ) ;
#14031 = ADVANCED_FACE ( 'NONE', ( #14883 ), #16927, .F. ) ;
#14032 = ORIENTED_EDGE ( 'NONE', *, *, #10021, .T. ) ;
#14033 = B_SPLINE_CURVE_WITH_KNOTS ( 'NONE', 3,
 ( #12820, #535, #14454, #5569, #21516, #2369, #19794, #19584 ),
 .UNSPECIFIED., .F., .F.,
 ( 4, 2, 2, 4 ),
 ( 0.005257893453559830781, 0.006567392922673201752, 0.007876892391786571856, 0.01049589133001331553 ),
 .UNSPECIFIED. ) ;
#14034 = FACE_BOUND ( 'NONE', #4289, .T. ) ;
#14035 = DIRECTION ( 'NONE',  ( 5.440186201345785633E-18, 1.000000000000000000, 1.334940939666367878E-17 ) ) ;
#14036 = CIRCLE ( 'NONE', #4832, 110.5000000000000142 ) ;
#14037 = VERTEX_POINT ( 'NONE', #15097 ) ;
#14038 = VECTOR ( 'NONE', #14702, 1000.000000000000114 ) ;
#14039 = CIRCLE ( 'NONE', #12928, 6.499999999999998224 ) ;
#14040 = CARTESIAN_POINT ( 'NONE',  ( 19.92486830831109046, 168.5282407225510326, 309.6860031901712205 ) ) ;
#14041 = ORIENTED_EDGE ( 'NONE', *, *, #2422, .F. ) ;
#14042 = CARTESIAN_POINT ( 'NONE',  ( -9.646142312030676180, 81.85301533877171209, -93.71525484045396581 ) ) ;
#14043 = CARTESIAN_POINT ( 'NONE',  ( -89.85464669586853859, 88.91429508965254058, 52.20121630638777077 ) ) ;
#14044 = AXIS2_PLACEMENT_3D ( 'NONE', #13117, #16576, #21911 ) ;
#14045 = VERTEX_POINT ( 'NONE', #1192 ) ;
#14046 = EDGE_CURVE ( 'NONE', #4037, #14965, #21933, .T. ) ;
#14047 = EDGE_LOOP ( 'NONE', ( #22100, #3128, #9702, #20306, #7068 ) ) ;
#14048 = CARTESIAN_POINT ( 'NONE',  ( -37.16746371568343932, 165.4537260709361135, 268.7306821537931683 ) ) ;
#14049 = DIRECTION ( 'NONE',  ( -7.125109674243555432E-05, 0.9999848031710253382, -0.005512562950850175003 ) ) ;
#14050 = ORIENTED_EDGE ( 'NONE', *, *, #15024, .T. ) ;
#14051 = DIRECTION ( 'NONE',  ( 7.125109674160258889E-05, -0.9999848031710252272, 0.005512562950849897447 ) ) ;
#14052 = AXIS2_PLACEMENT_3D ( 'NONE', #22551, #3516, #305 ) ;
#14053 = CARTESIAN_POINT ( 'NONE',  ( 82.15928189060839770, 75.11374352463818127, 3.586303559386837314 ) ) ;
#14054 = AXIS2_PLACEMENT_3D ( 'NONE', #954, #14525, #7601 ) ;
#14055 = CARTESIAN_POINT ( 'NONE',  ( -164.0000000000000000, 2.000000000000000000, -7.999999999999979572 ) ) ;
#14056 = VERTEX_POINT ( 'NONE', #6227 ) ;
#14057 = CARTESIAN_POINT ( 'NONE',  ( 20.02943147455619410, 184.4085440663593545, 276.4201140974324744 ) ) ;
#14058 = ORIENTED_EDGE ( 'NONE', *, *, #8215, .F. ) ;
#14059 = FACE_OUTER_BOUND ( 'NONE', #301, .T. ) ;
#14060 = CARTESIAN_POINT ( 'NONE',  ( -74.88934953599625999, 74.99999364505980282, 1.298876317593433916 ) ) ;
#14061 = CARTESIAN_POINT ( 'NONE',  ( -28.05907253792918610, 324.1127586016892224, 316.5723599207789789 ) ) ;
#14062 = DIRECTION ( 'NONE',  ( 0.01292414190464131682, 0.000000000000000000, 0.9999164797902017066 ) ) ;
#14063 = ADVANCED_FACE ( 'NONE', ( #8188 ), #15580, .T. ) ;
#14064 = VECTOR ( 'NONE', #13324, 999.9999999999998863 ) ;
#14065 = CARTESIAN_POINT ( 'NONE',  ( -162.0000000000000000, 0.000000000000000000, -53.76161406891256433 ) ) ;
#14066 = CARTESIAN_POINT ( 'NONE',  ( -56.88982296092818558, 126.2575686056375304, 47.57983110662539161 ) ) ;
#14067 = CARTESIAN_POINT ( 'NONE',  ( 104.8611102782643343, 70.00000000000000000, -33.22898942131121913 ) ) ;
#14068 = EDGE_LOOP ( 'NONE', ( #9490, #17389, #19099 ) ) ;
#14069 = DIRECTION ( 'NONE',  ( 7.125109674081160920E-05, -0.9999848031710253382, 0.005512562950849312846 ) ) ;
#14070 = ORIENTED_EDGE ( 'NONE', *, *, #2338, .T. ) ;
#14071 = AXIS2_PLACEMENT_3D ( 'NONE', #7420, #14337, #19252 ) ;
#14072 = ORIENTED_EDGE ( 'NONE', *, *, #832, .T. ) ;
#14073 = EDGE_LOOP ( 'NONE', ( #20774, #2600, #14475, #1388 ) ) ;
#14074 = VECTOR ( 'NONE', #6624, 1000.000000000000000 ) ;
#14075 = UNCERTAINTY_MEASURE_WITH_UNIT (LENGTH_MEASURE( 1.000000000000000082E-05 ), #5329, 'distance_accuracy_value', 'NONE');
#14076 = CARTESIAN_POINT ( 'NONE',  ( 17.35534499068185710, 186.7833359346272175, 309.5258091127471971 ) ) ;
#14077 = ORIENTED_EDGE ( 'NONE', *, *, #19865, .T. ) ;
#14078 = EDGE_CURVE ( 'NONE', #3399, #4461, #4497, .T. ) ;
#14079 = DIRECTION ( 'NONE',  ( 7.125109674161246868E-05, -0.9999848031710252272, 0.005512562950850154186 ) ) ;
#14080 = FACE_OUTER_BOUND ( 'NONE', #7247, .T. ) ;
#14081 = EDGE_CURVE ( 'NONE', #21571, #5484, #20876, .T. ) ;
#14082 = DIRECTION ( 'NONE',  ( 7.125109674364534776E-05, -0.9999848031710252272, 0.005512562950849704893 ) ) ;
#14083 = VECTOR ( 'NONE', #11988, 999.9999999999998863 ) ;
#14084 = FACE_OUTER_BOUND ( 'NONE', #16564, .T. ) ;
#14085 = CYLINDRICAL_SURFACE ( 'NONE', #7845, 3.399999999999986144 ) ;
#14086 =( LENGTH_UNIT ( ) NAMED_UNIT ( * ) SI_UNIT ( .MILLI., .METRE. ) );
#14087 = CARTESIAN_POINT ( 'NONE',  ( 83.04875907314333006, 75.15446773302494421, -6.489993662301849930 ) ) ;
#14088 = CARTESIAN_POINT ( 'NONE',  ( 20.29114497646528648, 182.2714854321924918, 311.7131426610552012 ) ) ;
#14089 = CONICAL_SURFACE ( 'NONE', #12258, 5.000000000000023981, 0.7853981633974460586 ) ;
#14090 = CARTESIAN_POINT ( 'NONE',  ( 92.18978923775409839, 77.29775901949989247, 29.08785173819693881 ) ) ;
#14091 = AXIS2_PLACEMENT_3D ( 'NONE', #5684, #18127, #14565 ) ;
#14092 = CARTESIAN_POINT ( 'NONE',  ( 89.33746586332900108, 79.97654757638647993, 29.19326486971733914 ) ) ;
#14093 = CARTESIAN_POINT ( 'NONE',  ( 91.62437796271727564, 95.71196945526500599, 60.86849236629024062 ) ) ;
#14094 = DIRECTION ( 'NONE',  ( -0.01292414190464130641, 8.584198644008937464E-16, -0.9999164797902015955 ) ) ;
#14095 = CARTESIAN_POINT ( 'NONE',  ( -11.19281454843939194, 155.5569384583423300, 101.2152518466410243 ) ) ;
#14096 = ORIENTED_EDGE ( 'NONE', *, *, #9360, .F. ) ;
#14097 = VECTOR ( 'NONE', #259, 1000.000000000000000 ) ;
#14098 = CARTESIAN_POINT ( 'NONE',  ( -92.30767208729371021, 77.25770192717985196, -29.02102379856271952 ) ) ;
#14099 = ORIENTED_EDGE ( 'NONE', *, *, #11734, .F. ) ;
#14100 = AXIS2_PLACEMENT_3D ( 'NONE', #17675, #15962, #7197 ) ;
#14101 = ADVANCED_FACE ( 'NONE', ( #6356 ), #5260, .T. ) ;
#14102 = CARTESIAN_POINT ( 'NONE',  ( -70.44022362938049753, 70.80424004364375890, -84.48783506240401664 ) ) ;
#14103 = DIRECTION ( 'NONE',  ( -0.01292394549866745720, -0.005513023399720816918, -0.9999012842304692006 ) ) ;
#14104 = PRODUCT_DEFINITION_CONTEXT ( 'detailed design', #4983, 'design' ) ;
#14105 = FACE_OUTER_BOUND ( 'NONE', #18195, .T. ) ;
#14106 = APPLICATION_CONTEXT ( 'automotive_design' ) ;
#14107 = DIRECTION ( 'NONE',  ( 0.9999164797902017066, 6.965998958219365988E-18, -0.01292414190464157356 ) ) ;
#14108 = ORIENTED_EDGE ( 'NONE', *, *, #16537, .F. ) ;
#14109 = DIRECTION ( 'NONE',  ( -2.025474946048326158E-22, 1.000000000000000000, -1.876735158486679638E-22 ) ) ;
#14110 = ORIENTED_EDGE ( 'NONE', *, *, #14479, .T. ) ;
#14111 = VERTEX_POINT ( 'NONE', #7011 ) ;
#14112 = VECTOR ( 'NONE', #13873, 1000.000000000000000 ) ;
#14113 = FACE_BOUND ( 'NONE', #17339, .T. ) ;
#14114 = CARTESIAN_POINT ( 'NONE',  ( 52.39275651943277268, 106.8510597072923218, 70.21618947625844953 ) ) ;
#14115 = CARTESIAN_POINT ( 'NONE',  ( -9.899470319389305217, 187.6214926260726656, 321.1548253226370093 ) ) ;
#14116 = CARTESIAN_POINT ( 'NONE',  ( -88.82263333796721838, 169.9999999999999716, 1.148052203164671159 ) ) ;
#14117 = CIRCLE ( 'NONE', #17060, 4.500000000000006217 ) ;
#14118 = VERTEX_POINT ( 'NONE', #1843 ) ;
#14119 = CARTESIAN_POINT ( 'NONE',  ( -15.15257079676713126, 179.5546631012716432, 315.4103692381972905 ) ) ;
#14120 = TOROIDAL_SURFACE ( 'NONE', #21439, 77.00000000000002842, 2.000000000000000000 ) ;
#14121 = EDGE_CURVE ( 'NONE', #12879, #10577, #895, .T. ) ;
#14122 = CYLINDRICAL_SURFACE ( 'NONE', #11393, 3.099999999999998757 ) ;
#14123 = CARTESIAN_POINT ( 'NONE',  ( 15.86053680860744564, 168.0563658420342961, 307.9314113524436038 ) ) ;
#14124 = CARTESIAN_POINT ( 'NONE',  ( -15.04605271383937470, 179.9046364190501208, 313.1717202347408033 ) ) ;
#14125 = ORIENTED_EDGE ( 'NONE', *, *, #20279, .F. ) ;
#14126 = CARTESIAN_POINT ( 'NONE',  ( 20.56772423864910948, 182.0615390744364106, 316.0167400927113590 ) ) ;
#14127 = DIRECTION ( 'NONE',  ( -0.01292394549866738782, -0.005513023399720468239, -0.9999012842304692006 ) ) ;
#14128 = VECTOR ( 'NONE', #17275, 1000.000000000000000 ) ;
#14129 = EDGE_CURVE ( 'NONE', #19370, #14056, #7, .T. ) ;
#14130 = DIRECTION ( 'NONE',  ( 0.9232306267972777425, 0.000000000000000000, -0.3842462878721220054 ) ) ;
#14131 = CONTEXT_DEPENDENT_SHAPE_REPRESENTATION ( #12666, #6992 ) ;
#14132 = PLANE ( 'NONE',  #7499 ) ;
#14133 = ADVANCED_FACE ( 'NONE', ( #12320 ), #15215, .F. ) ;
#14134 = CIRCLE ( 'NONE', #21081, 2.000000000000001332 ) ;
#14135 = EDGE_CURVE ( 'NONE', #7464, #6252, #19297, .T. ) ;
#14136 = DIRECTION ( 'NONE',  ( 0.01292394549866733230, 0.005513023399720419666, 0.9999012842304692006 ) ) ;
#14137 = DIRECTION ( 'NONE',  ( -0.9506032891036972909, 0.3102281881984321754, 0.01057629388542893900 ) ) ;
#14138 = CARTESIAN_POINT ( 'NONE',  ( 38.92395541352284738, 91.17157287525387233, -83.51003349877244375 ) ) ;
#14139 = DIRECTION ( 'NONE',  ( 0.5847225553467816361, 0.5805244408402039369, 0.5666488391022245219 ) ) ;
#14140 = ORIENTED_EDGE ( 'NONE', *, *, #2526, .T. ) ;
#14141 = VERTEX_POINT ( 'NONE', #17212 ) ;
#14142 = DIRECTION ( 'NONE',  ( -0.006350819331213198964, 0.8709385446395360164, -0.4913509118287961996 ) ) ;
#14143 = CARTESIAN_POINT ( 'NONE',  ( -50.61043681403349837, 112.8347543081579403, -43.53505773252739175 ) ) ;
#14144 = ORIENTED_EDGE ( 'NONE', *, *, #9067, .F. ) ;
#14145 = CARTESIAN_POINT ( 'NONE',  ( 2.809107650776963450, 87.00000000000001421, -86.95587516435855946 ) ) ;
#14146 = VERTEX_POINT ( 'NONE', #16889 ) ;
#14147 = SHAPE_REPRESENTATION_RELATIONSHIP ( 'NONE' , 'NONE' ,  #9590, #3337 ) ;
#14148 = DIRECTION ( 'NONE',  ( -0.4397038457472313144, 0.000000000000000000, -0.8981428216242086648 ) ) ;
#14149 = AXIS2_PLACEMENT_3D ( 'NONE', #18521, #955, #4366 ) ;
#14150 = FACE_OUTER_BOUND ( 'NONE', #120, .T. ) ;
#14151 = CARTESIAN_POINT ( 'NONE',  ( -93.62421092229762110, 72.00000000000000000, -60.84264408248100864 ) ) ;
#14152 = ADVANCED_FACE ( 'NONE', ( #13339 ), #22133, .T. ) ;
#14153 = ORIENTED_EDGE ( 'NONE', *, *, #18593, .T. ) ;
#14154 = CYLINDRICAL_SURFACE ( 'NONE', #5619, 3.399999999999991918 ) ;
#14155 = DIRECTION ( 'NONE',  ( 0.1351880940536942799, -0.9908129862407182298, 0.003715578404455081168 ) ) ;
#14156 = CARTESIAN_POINT ( 'NONE',  ( 16.07150438106780399, 168.1329592171555305, 320.9330071493605487 ) ) ;
#14157 = EDGE_CURVE ( 'NONE', #16867, #1653, #10800, .T. ) ;
#14158 = ORIENTED_EDGE ( 'NONE', *, *, #17570, .F. ) ;
#14159 = PLANE ( 'NONE',  #4702 ) ;
#14160 = CARTESIAN_POINT ( 'NONE',  ( -89.95235262792742503, 87.80448589959429739, 50.90690957908749681 ) ) ;
#14161 = VECTOR ( 'NONE', #12092, 1000.000000000000114 ) ;
#14162 = EDGE_CURVE ( 'NONE', #345, #2627, #22512, .T. ) ;
#14164 = ORIENTED_EDGE ( 'NONE', *, *, #20137, .T. ) ;
#14163 = ORIENTED_EDGE ( 'NONE', *, *, #21880, .F. ) ;
#14165 = EDGE_CURVE ( 'NONE', #20879, #44, #464, .T. ) ;
#14166 = ORIENTED_EDGE ( 'NONE', *, *, #14591, .T. ) ;
#14167 = LINE ( 'NONE', #7241, #70 ) ;
#14168 = EDGE_CURVE ( 'NONE', #11287, #18203, #8584, .T. ) ;
#14169 = DIRECTION ( 'NONE',  ( -0.9999164797902015955, -6.965998958219364448E-18, 0.01292414190464157182 ) ) ;
#14170 = CYLINDRICAL_SURFACE ( 'NONE', #11294, 4.200000000000005507 ) ;
#14171 = LINE ( 'NONE', #17607, #14161 ) ;
#14172 = DIRECTION ( 'NONE',  ( -0.01292394549866740169, -0.005513023399721277487, -0.9999012842304693116 ) ) ;
#14173 = ORIENTED_EDGE ( 'NONE', *, *, #8180, .T. ) ;
#14174 = ORIENTED_EDGE ( 'NONE', *, *, #15743, .T. ) ;
#14175 = CARTESIAN_POINT ( 'NONE',  ( 71.61338682171094661, 92.58578643762700722, 83.49564556265194426 ) ) ;
#14176 = CARTESIAN_POINT ( 'NONE',  ( -45.67464185259402853, 168.2105890667581605, -51.90496219196452188 ) ) ;
#14177 = CARTESIAN_POINT ( 'NONE',  ( -77.49583701682549020, 75.10299918630330751, -3.425180504331486908 ) ) ;
#14178 = CARTESIAN_POINT ( 'NONE',  ( -27.71828981744229381, 324.1286477571945284, 310.8524157770490888 ) ) ;
#14179 = EDGE_LOOP ( 'NONE', ( #1310, #10994, #2288, #21473 ) ) ;
#14180 = LINE ( 'NONE', #17395, #20930 ) ;
#14181 = EDGE_LOOP ( 'NONE', ( #4093, #15086, #18273, #17409, #6300 ) ) ;
#14182 = DIRECTION ( 'NONE',  ( -0.01292394549867042185, -0.005513023399725255208, -0.9999012842304693116 ) ) ;
#14183 = FILL_AREA_STYLE_COLOUR ( '', #17813 ) ;
#14184 = DIRECTION ( 'NONE',  ( 2.449293598294706414E-16, 0.000000000000000000, 1.000000000000000000 ) ) ;
#14185 = AXIS2_PLACEMENT_3D ( 'NONE', #8821, #20887, #13896 ) ;
#14186 = DIRECTION ( 'NONE',  ( -0.01292394549866738782, -0.005513023399720468239, -0.9999012842304692006 ) ) ;
#14187 = ORIENTED_EDGE ( 'NONE', *, *, #17013, .F. ) ;
#14188 = PRODUCT_DEFINITION_SHAPE ( 'NONE', 'NONE',  #22698 ) ;
#14189 = EDGE_CURVE ( 'NONE', #20596, #12054, #19269, .T. ) ;
#14190 = CARTESIAN_POINT ( 'NONE',  ( -6.866741853946069618, 164.5525188853477232, 83.72578275117199098 ) ) ;
#14191 = ORIENTED_EDGE ( 'NONE', *, *, #18375, .F. ) ;
#14192 = ORIENTED_EDGE ( 'NONE', *, *, #14900, .F. ) ;
#14193 = EDGE_LOOP ( 'NONE', ( #20332, #2467, #5998, #7029, #3801 ) ) ;
#14194 = CARTESIAN_POINT ( 'NONE',  ( -58.84901841222320229, 118.8937358571614453, 163.0286266904498405 ) ) ;
#14195 = ORIENTED_EDGE ( 'NONE', *, *, #14189, .T. ) ;
#14196 = EDGE_CURVE ( 'NONE', #21200, #3357, #7963, .T. ) ;
#14197 = ADVANCED_FACE ( 'NONE', ( #19034 ), #18523, .T. ) ;
#14198 = DIRECTION ( 'NONE',  ( -0.4397038457472354778, 0.000000000000000000, -0.8981428216242066664 ) ) ;
#14199 = DIRECTION ( 'NONE',  ( -0.009188991635466048358, 0.7031977391749438810, -0.7109349492407661675 ) ) ;
#14200 = CARTESIAN_POINT ( 'NONE',  ( -91.00106904273528130, 70.29040131071506892, 61.79648398638329354 ) ) ;
#14201 = CARTESIAN_POINT ( 'NONE',  ( 106.1636641531657972, 79.04398536104962147, -28.79715981783310497 ) ) ;
#14202 = DIRECTION ( 'NONE',  ( -0.01292394549866745720, -0.005513023399720816918, -0.9999012842304692006 ) ) ;
#14203 = PRODUCT_DEFINITION_SHAPE ( 'NONE', 'NONE',  #13947 ) ;
#14204 = FILL_AREA_STYLE ('',( #10399 ) ) ;
#14205 = CARTESIAN_POINT ( 'NONE',  ( 77.34116450907883689, 75.17093467388001216, -6.697014498691808981 ) ) ;
#14206 = CARTESIAN_POINT ( 'NONE',  ( 13.11950053790673998, 190.3195187405954130, 307.8718610784719658 ) ) ;
#14207 = CARTESIAN_POINT ( 'NONE',  ( 91.37189824458509690, 79.16991425845409935, 26.65847270750105480 ) ) ;
#14208 = LINE ( 'NONE', #12248, #7723 ) ;
#14209 = ORIENTED_EDGE ( 'NONE', *, *, #2341, .T. ) ;
#14210 = EDGE_CURVE ( 'NONE', #5236, #6260, #21779, .T. ) ;
#14211 = DIRECTION ( 'NONE',  ( -0.01246513159389404414, -0.2641402835564772844, -0.9644037178988117409 ) ) ;
#14212 = PLANE ( 'NONE',  #11785 ) ;
#14213 = ADVANCED_FACE ( 'NONE', ( #2238 ), #15736, .T. ) ;
#14214 = EDGE_LOOP ( 'NONE', ( #15772, #1476, #6942 ) ) ;
#14215 = DIRECTION ( 'NONE',  ( 0.01292414190464131335, 0.000000000000000000, 0.9999164797902017066 ) ) ;
#14216 = ORIENTED_EDGE ( 'NONE', *, *, #612, .T. ) ;
#14217 = LINE ( 'NONE', #3270, #1129 ) ;
#14218 = DIRECTION ( 'NONE',  ( 7.125109674160258889E-05, -0.9999848031710252272, 0.005512562950849897447 ) ) ;
#14219 = LINE ( 'NONE', #1795, #17011 ) ;
#14220 = DIRECTION ( 'NONE',  ( 0.01292414190464131335, 1.902755938799530239E-22, 0.9999164797902015955 ) ) ;
#14221 = DIRECTION ( 'NONE',  ( 1.000000000000000000, -0.000000000000000000, 0.000000000000000000 ) ) ;
#14222 = ORIENTED_EDGE ( 'NONE', *, *, #14369, .F. ) ;
#14223 = CARTESIAN_POINT ( 'NONE',  ( 3.316624388958365088, 166.4147108432491109, 256.6009726804241495 ) ) ;
#14224 = ORIENTED_EDGE ( 'NONE', *, *, #19016, .T. ) ;
#14225 = VERTEX_POINT ( 'NONE', #11096 ) ;
#14226 = CARTESIAN_POINT ( 'NONE',  ( -53.12394241931270500, 114.6366640169135849, 162.3035455873394426 ) ) ;
#14227 = AXIS2_PLACEMENT_3D ( 'NONE', #3258, #10284, #13206 ) ;
#14228 = CARTESIAN_POINT ( 'NONE',  ( 51.30310378538536042, 107.3244244979011057, 69.70064189502821250 ) ) ;
#14229 = EDGE_LOOP ( 'NONE', ( #2419, #17072, #485, #9125 ) ) ;
#14230 = CARTESIAN_POINT ( 'NONE',  ( -10.25967351461796362, 187.2843258730522393, 321.1153754285980426 ) ) ;
#14231 = CARTESIAN_POINT ( 'NONE',  ( -90.47544334247993447, 78.08471258854567054, 32.66922098773510186 ) ) ;
#14232 = DIRECTION ( 'NONE',  ( 0.000000000000000000, 0.000000000000000000, 1.000000000000000000 ) ) ;
#14233 = EDGE_LOOP ( 'NONE', ( #229, #13432, #14295, #9335 ) ) ;
#14234 = CARTESIAN_POINT ( 'NONE',  ( -10.02117361870881851, 187.8727420016839176, 308.1601407300097435 ) ) ;
#14235 = EDGE_CURVE ( 'NONE', #21699, #14111, #3642, .T. ) ;
#14236 = CARTESIAN_POINT ( 'NONE',  ( -58.43812057966402307, 118.9192529882355842, 167.6521505577929645 ) ) ;
#14237 = CARTESIAN_POINT ( 'NONE',  ( 16.44044660180618678, 168.1228407995204179, 307.9702792283749773 ) ) ;
#14238 = CARTESIAN_POINT ( 'NONE',  ( -14.25139930150079515, 179.7940826540526871, 318.1440894004308007 ) ) ;
#14239 = CARTESIAN_POINT ( 'NONE',  ( 17.86254487970774463, 184.6173340417515760, 321.1453017134867309 ) ) ;
#14240 = VERTEX_POINT ( 'NONE', #12817 ) ;
#14241 = AXIS2_PLACEMENT_3D ( 'NONE', #11963, #15313, #13799 ) ;
#14242 = DIRECTION ( 'NONE',  ( -0.000000000000000000, -1.000000000000000000, -0.000000000000000000 ) ) ;
#14243 = CARTESIAN_POINT ( 'NONE',  ( 38.37734285175992710, 94.19957547781432083, 82.31130495470515029 ) ) ;
#14244 = CARTESIAN_POINT ( 'NONE',  ( -55.33804461215960657, 114.2193244133317904, 167.6379947637574617 ) ) ;
#14245 = DIRECTION ( 'NONE',  ( 0.9232306267972774094, 0.000000000000000000, -0.3842462878721227826 ) ) ;
#14246 = CARTESIAN_POINT ( 'NONE',  ( 51.38234815825343560, 111.9218655255082382, -48.12259961501337102 ) ) ;
#14247 = ORIENTED_EDGE ( 'NONE', *, *, #20397, .F. ) ;
#14248 = TOROIDAL_SURFACE ( 'NONE', #4315, 124.0000000000000000, 2.000000000000000000 ) ;
#14249 = ORIENTED_EDGE ( 'NONE', *, *, #18616, .T. ) ;
#14250 = DIRECTION ( 'NONE',  ( 7.125109674403277385E-05, -0.9999848031710253382, 0.005512562950848281552 ) ) ;
#14251 = CARTESIAN_POINT ( 'NONE',  ( -52.26459910193298697, 113.4816418249607750, -43.51724397679114276 ) ) ;
#14252 = ORIENTED_EDGE ( 'NONE', *, *, #2357, .F. ) ;
#14253 = CARTESIAN_POINT ( 'NONE',  ( 79.99331838321626265, 102.0000000000000000, -6.033931352371315171 ) ) ;
#14254 = ORIENTED_EDGE ( 'NONE', *, *, #16541, .T. ) ;
#14255 = DIRECTION ( 'NONE',  ( 0.01292414190464131508, 1.902755938799530474E-22, 0.9999164797902017066 ) ) ;
#14256 = DIRECTION ( 'NONE',  ( -0.9999164797902017066, -2.001050586450180576E-22, 0.01292414190464044946 ) ) ;
#14257 = FACE_BOUND ( 'NONE', #21338, .T. ) ;
#14258 = CIRCLE ( 'NONE', #13882, 2.000000000000007550 ) ;
#14259 = FACE_OUTER_BOUND ( 'NONE', #3119, .T. ) ;
#14260 = CARTESIAN_POINT ( 'NONE',  ( 11.78612559536878734, 143.6154693132956766, 275.8089238432258412 ) ) ;
#14261 = B_SPLINE_CURVE_WITH_KNOTS ( 'NONE', 3,
 ( #19049, #6768, #15749, #1611, #20665, #11956 ),
 .UNSPECIFIED., .F., .F.,
 ( 4, 2, 4 ),
 ( 0.01452727543195645593, 0.01715716534226980478, 0.01978705525258315362 ),
 .UNSPECIFIED. ) ;
#14262 = EDGE_CURVE ( 'NONE', #5442, #18327, #17062, .T. ) ;
#14263 = CARTESIAN_POINT ( 'NONE',  ( -3.492210504507778257, 326.9352113893252749, 319.7943972700559243 ) ) ;
#14264 = EDGE_LOOP ( 'NONE', ( #19441, #11651, #17445 ) ) ;
#14265 = CARTESIAN_POINT ( 'NONE',  ( 42.91324393340197219, 106.8060942374655156, 70.38454212103849272 ) ) ;
#14266 = CARTESIAN_POINT ( 'NONE',  ( -88.16771777505866226, 88.62629760424535164, 52.53058358910858061 ) ) ;
#14267 = ORIENTED_EDGE ( 'NONE', *, *, #10040, .T. ) ;
#14268 = ADVANCED_FACE ( 'NONE', ( #19790 ), #9244, .T. ) ;
#14269 = ORIENTED_EDGE ( 'NONE', *, *, #2892, .F. ) ;
#14270 = CARTESIAN_POINT ( 'NONE',  ( 163.9999999999992610, 18.00000000000000355, 53.76161406891480965 ) ) ;
#14271 = ADVANCED_FACE ( 'NONE', ( #19380 ), #17338, .F. ) ;
#14272 = PLANE ( 'NONE',  #22053 ) ;
#14273 = DIRECTION ( 'NONE',  ( 7.125109674381880655E-05, -0.9999848031710253382, 0.005512562950849702291 ) ) ;
#14274 = DIRECTION ( 'NONE',  ( -0.9999164797902015955, -2.001050586450178695E-22, 0.01292414190464131335 ) ) ;
#14275 = LINE ( 'NONE', #1643, #19210 ) ;
#14276 = ORIENTED_EDGE ( 'NONE', *, *, #9579, .T. ) ;
#14277 = ADVANCED_FACE ( 'NONE', ( #21515 ), #21107, .F. ) ;
#14278 = FACE_OUTER_BOUND ( 'NONE', #18931, .T. ) ;
#14279 = ORIENTED_EDGE ( 'NONE', *, *, #7356, .F. ) ;
#14280 = CARTESIAN_POINT ( 'NONE',  ( 394.9504264446939032, 92.58578643762714933, -89.52608615654102664 ) ) ;
#14281 = DIRECTION ( 'NONE',  ( -0.01292394549866738782, -0.005513023399720700692, -0.9999012842304693116 ) ) ;
#14282 = CARTESIAN_POINT ( 'NONE',  ( -2.476119979858705467, 190.7342627770796355, 256.5417576885990343 ) ) ;
#14283 = CARTESIAN_POINT ( 'NONE',  ( -27.47457004210972897, 324.1549168750700574, 310.4553055122309502 ) ) ;
#14284 = VECTOR ( 'NONE', #1808, 1000.000000000000000 ) ;
#14285 = VERTEX_POINT ( 'NONE', #10661 ) ;
#14286 = CARTESIAN_POINT ( 'NONE',  ( -105.4390993001728276, 77.44561610140179653, 31.34641640711149790 ) ) ;
#14287 = ORIENTED_EDGE ( 'NONE', *, *, #15355, .T. ) ;
#14288 = FACE_OUTER_BOUND ( 'NONE', #20784, .T. ) ;
#14289 = DIRECTION ( 'NONE',  ( 0.01292394549866731843, 0.005513023399720594006, 0.9999012842304693116 ) ) ;
#14290 =( GEOMETRIC_REPRESENTATION_CONTEXT ( 3 ) GLOBAL_UNCERTAINTY_ASSIGNED_CONTEXT ( ( #11368 ) ) GLOBAL_UNIT_ASSIGNED_CONTEXT ( ( #15216, #3000, #6224 ) ) REPRESENTATION_CONTEXT ( 'NONE', 'WORKASPACE' ) );
#14291 = CARTESIAN_POINT ( 'NONE',  ( 104.9795361740884090, 70.06102247219406820, -32.85291587203231245 ) ) ;
#14292 = ADVANCED_FACE ( 'NONE', ( #3535 ), #7531, .T. ) ;
#14293 = ORIENTED_EDGE ( 'NONE', *, *, #20841, .F. ) ;
#14294 = EDGE_CURVE ( 'NONE', #14473, #8505, #6859, .T. ) ;
#14295 = ORIENTED_EDGE ( 'NONE', *, *, #3526, .T. ) ;
#14296 = DIRECTION ( 'NONE',  ( -0.01292394549866741384, -0.005513023399720270480, -0.9999012842304693116 ) ) ;
#14297 = ORIENTED_EDGE ( 'NONE', *, *, #10409, .T. ) ;
#14298 = ORIENTED_EDGE ( 'NONE', *, *, #6738, .T. ) ;
#14299 = ORIENTED_EDGE ( 'NONE', *, *, #12045, .F. ) ;
#14300 = EDGE_CURVE ( 'NONE', #10951, #6286, #1818, .T. ) ;
#14301 = UNCERTAINTY_MEASURE_WITH_UNIT (LENGTH_MEASURE( 1.000000000000000082E-05 ), #12616, 'distance_accuracy_value', 'NONE');
#14302 = CARTESIAN_POINT ( 'NONE',  ( 19.75650998535411063, 183.7491368459512842, 312.9879496513954678 ) ) ;
#14303 = CIRCLE ( 'NONE', #16866, 5.100000000000000533 ) ;
#14304 = EDGE_LOOP ( 'NONE', ( #17441, #21456, #19600 ) ) ;
#14305 = EDGE_CURVE ( 'NONE', #19636, #2746, #21932, .T. ) ;
#14306 = CARTESIAN_POINT ( 'NONE',  ( 49.42284594772163331, 139.7551263635817236, -44.97643735496247785 ) ) ;
#14307 = ADVANCED_BREP_SHAPE_REPRESENTATION ( '', ( #17112, #6292 ), #10694 ) ;
#14308 = VECTOR ( 'NONE', #20411, 1000.000000000000000 ) ;
#14309 = CARTESIAN_POINT ( 'NONE',  ( 39.46073478354046671, 96.01222662467367286, -42.85086330523944298 ) ) ;
#14310 = CARTESIAN_POINT ( 'NONE',  ( -11.41931823208222774, 147.4996510494855215, 278.6483820114981995 ) ) ;
#14311 = EDGE_CURVE ( 'NONE', #1581, #3464, #21742, .T. ) ;
#14312 = FACE_OUTER_BOUND ( 'NONE', #6527, .T. ) ;
#14313 = CARTESIAN_POINT ( 'NONE',  ( -38.48616300399660162, 94.99421645999460395, 83.38067543124275005 ) ) ;
#14314 = EDGE_CURVE ( 'NONE', #883, #15636, #8958, .T. ) ;
#14315 = ORIENTED_EDGE ( 'NONE', *, *, #4672, .T. ) ;
#14316 = CARTESIAN_POINT ( 'NONE',  ( -90.04901853436439296, 75.26362638851092868, 71.79194879392322548 ) ) ;
#14317 = CARTESIAN_POINT ( 'NONE',  ( 86.23745778024132846, 74.99999999999998579, -1.527744779571642342 ) ) ;
#14318 = CARTESIAN_POINT ( 'NONE',  ( 16.09649071154515099, 185.6410692198624020, 306.2537067563579285 ) ) ;
#14319 = CARTESIAN_POINT ( 'NONE',  ( 91.23603883849618512, 78.43035437438882695, 30.82342686631244888 ) ) ;
#14320 = CARTESIAN_POINT ( 'NONE',  ( -84.57230515545194294, 104.9999999999999858, -70.33944174062779098 ) ) ;
#14321 = CIRCLE ( 'NONE', #19057, 2.000000000000001332 ) ;
#14322 = CIRCLE ( 'NONE', #20511, 3.999999999999999556 ) ;
#14323 = EDGE_CURVE ( 'NONE', #15796, #9955, #1099, .T. ) ;
#14324 = CARTESIAN_POINT ( 'NONE',  ( -8.637836329777936584, 185.8852932021121376, 322.1857653656461480 ) ) ;
#14325 = DIRECTION ( 'NONE',  ( 0.9999164797902017066, 2.001050586450178695E-22, -0.01292414190464131508 ) ) ;
#14326 = AXIS2_PLACEMENT_3D ( 'NONE', #442, #9388, #10890 ) ;
#14327 = ORIENTED_EDGE ( 'NONE', *, *, #16442, .T. ) ;
#14328 = LINE ( 'NONE', #3852, #13527 ) ;
#14329 = ORIENTED_EDGE ( 'NONE', *, *, #19877, .F. ) ;
#14330 = ORIENTED_EDGE ( 'NONE', *, *, #8072, .T. ) ;
#14331 = CARTESIAN_POINT ( 'NONE',  ( -38.46180957136326128, 93.08398165842332617, 84.42015501544445044 ) ) ;
#14332 = FILL_AREA_STYLE ('',( #7293 ) ) ;
#14333 = AXIS2_PLACEMENT_3D ( 'NONE', #18789, #1453, #22538 ) ;
#14334 = ORIENTED_EDGE ( 'NONE', *, *, #11050, .F. ) ;
#14335 = CARTESIAN_POINT ( 'NONE',  ( -64.99457118636313169, 170.0000000000000284, 0.8400692238016805868 ) ) ;
#14336 = AXIS2_PLACEMENT_3D ( 'NONE', #22402, #10149, #1320 ) ;
#14337 = DIRECTION ( 'NONE',  ( -7.125109674161231961E-05, 0.9999848031710252272, -0.005512562950850142043 ) ) ;
#14338 = ADVANCED_FACE ( 'NONE', ( #7972 ), #10820, .T. ) ;
#14339 = ORIENTED_EDGE ( 'NONE', *, *, #3771, .F. ) ;
#14340 = CARTESIAN_POINT ( 'NONE',  ( -162.0000000000000000, 2.000000000000000000, 0.000000000000000000 ) ) ;
#14341 = EDGE_LOOP ( 'NONE', ( #18959, #1353, #17666, #1145, #344 ) ) ;
#14342 = ORIENTED_EDGE ( 'NONE', *, *, #4262, .F. ) ;
#14343 = PRODUCT_DEFINITION_FORMATION_WITH_SPECIFIED_SOURCE ( 'ANY', '', #8650, .NOT_KNOWN. ) ;
#14344 = CARTESIAN_POINT ( 'NONE',  ( -45.15312007873931321, 180.5703843163154545, 257.1494065962392597 ) ) ;
#14345 = LINE ( 'NONE', #3630, #2580 ) ;
#14346 = DIRECTION ( 'NONE',  ( -0.6979091139780387865, 0.003898296230782335829, 0.7161757269782926816 ) ) ;
#14347 = AXIS2_PLACEMENT_3D ( 'NONE', #2146, #2042, #7554 ) ;
#14348 = CARTESIAN_POINT ( 'NONE',  ( -91.47655718793627955, 79.89818662653908632, 31.35069918968696712 ) ) ;
#14349 = CARTESIAN_POINT ( 'NONE',  ( -88.18368518054532501, 87.00751446224754204, 51.35601162712541168 ) ) ;
#14350 = EDGE_LOOP ( 'NONE', ( #15046, #5723, #3269, #5264 ) ) ;
#14351 = CARTESIAN_POINT ( 'NONE',  ( -15.03108941308168234, 179.9501653168765358, 313.0619997550173252 ) ) ;
#14352 = EDGE_LOOP ( 'NONE', ( #13528, #5598, #7044, #11125, #18947 ) ) ;
#14353 = EDGE_CURVE ( 'NONE', #5961, #3219, #14506, .T. ) ;
#14354 = EDGE_LOOP ( 'NONE', ( #18576, #1974, #3834, #7330 ) ) ;
#14355 = SPHERICAL_SURFACE ( 'NONE', #10273, 2.000000000000000000 ) ;
#14356 = CARTESIAN_POINT ( 'NONE',  ( -13.20095895536456609, 181.0966850513278814, 321.5989609326452978 ) ) ;
#14357 = AXIS2_PLACEMENT_3D ( 'NONE', #22314, #17183, #22211 ) ;
#14358 = AXIS2_PLACEMENT_3D ( 'NONE', #16255, #18191, #14527 ) ;
#14359 = CARTESIAN_POINT ( 'NONE',  ( 14.76142725739638273, 167.8843352801436026, 296.4488922160406332 ) ) ;
#14360 = AXIS2_PLACEMENT_3D ( 'NONE', #16211, #14368, #19278 ) ;
#14361 = DIRECTION ( 'NONE',  ( 0.9232306267972774094, 0.000000000000000000, -0.3842462878721226160 ) ) ;
#14362 = ORIENTED_EDGE ( 'NONE', *, *, #15691, .T. ) ;
#14363 = CARTESIAN_POINT ( 'NONE',  ( -9.472248412593195610, 81.99999999999998579, -86.53426659026914081 ) ) ;
#14364 = CIRCLE ( 'NONE', #389, 12.37020706055088759 ) ;
#14365 = CONTEXT_DEPENDENT_SHAPE_REPRESENTATION ( #11483, #15272 ) ;
#14366 = CARTESIAN_POINT ( 'NONE',  ( 19.43891449096291169, 175.6145212674599065, 111.2097777439524151 ) ) ;
#14367 = EDGE_CURVE ( 'NONE', #15447, #8963, #22142, .T. ) ;
#14368 = DIRECTION ( 'NONE',  ( 0.9999164797902017066, 2.001050586450178695E-22, -0.01292414190464131508 ) ) ;
#14369 = EDGE_CURVE ( 'NONE', #11822, #3438, #7871, .T. ) ;
#14370 = DIRECTION ( 'NONE',  ( 0.9999164797902015955, 6.965998958219364448E-18, -0.01292414190464157182 ) ) ;
#14371 = ORIENTED_EDGE ( 'NONE', *, *, #21105, .T. ) ;
#14372 = CARTESIAN_POINT ( 'NONE',  ( 39.40254987707581336, 92.58578643762697880, -84.93055112583749633 ) ) ;
#14373 = CARTESIAN_POINT ( 'NONE',  ( 79.92740525950247843, 75.13699351169599083, -6.133505399301336425 ) ) ;
#14374 = VECTOR ( 'NONE', #7625, 1000.000000000000000 ) ;
#14375 = CARTESIAN_POINT ( 'NONE',  ( -5.703700719415883746, 174.2634384100414593, 299.6785330862965679 ) ) ;
#14376 = EDGE_LOOP ( 'NONE', ( #7211, #7041, #11700, #6032, #13423 ) ) ;
#14377 = ORIENTED_EDGE ( 'NONE', *, *, #13218, .T. ) ;
#14378 = CARTESIAN_POINT ( 'NONE',  ( -39.42082737383933733, 91.17157287525387233, 83.51645567887779009 ) ) ;
#14380 = DIRECTION ( 'NONE',  ( -0.01292394549866740169, -0.005513023399719847208, -0.9999012842304693116 ) ) ;
#14379 = CARTESIAN_POINT ( 'NONE',  ( -64.28883878761490678, 83.29019440189556178, 55.44125366118054643 ) ) ;
#14381 = AXIS2_PLACEMENT_3D ( 'NONE', #15672, #1537, #17157 ) ;
#14382 = CARTESIAN_POINT ( 'NONE',  ( -41.14926644985963122, 168.6907664596094776, 35.14123791416483300 ) ) ;
#14383 = DIRECTION ( 'NONE',  ( 0.01292414190464131508, 0.000000000000000000, 0.9999164797902017066 ) ) ;
#14384 = ORIENTED_EDGE ( 'NONE', *, *, #963, .T. ) ;
#14385 = VERTEX_POINT ( 'NONE', #21851 ) ;
#14386 = CARTESIAN_POINT ( 'NONE',  ( 13.29718515720261607, 144.2203306461185264, 276.4281824851719875 ) ) ;
#14387 = MECHANICAL_DESIGN_GEOMETRIC_PRESENTATION_REPRESENTATION (  '', ( #1526 ), #7140 ) ;
#14388 = DIRECTION ( 'NONE',  ( 7.125109674160325297E-05, -0.9999848031710253382, 0.005512562950849327591 ) ) ;
#14389 = VERTEX_POINT ( 'NONE', #18444 ) ;
#14390 = LINE ( 'NONE', #19632, #15034 ) ;
#14391 = AXIS2_PLACEMENT_3D ( 'NONE', #3240, #6705, #13611 ) ;
#14392 = CARTESIAN_POINT ( 'NONE',  ( -90.00743053908078650, 87.70552466312305739, 50.96783830792826109 ) ) ;
#14393 = APPLICATION_PROTOCOL_DEFINITION ( 'draft international standard', 'automotive_design', 1998, #1916 ) ;
#14394 = AXIS2_PLACEMENT_3D ( 'NONE', #360, #15895, #10698 ) ;
#14396 = VERTEX_POINT ( 'NONE', #6145 ) ;
#14395 = EDGE_LOOP ( 'NONE', ( #5023, #4827, #15445, #19304 ) ) ;
#14397 = ORIENTED_EDGE ( 'NONE', *, *, #19865, .F. ) ;
#14398 = DIRECTION ( 'NONE',  ( -0.9910138020846641638, 0.1337596504095987238, 0.000000000000000000 ) ) ;
#14399 = AXIS2_PLACEMENT_3D ( 'NONE', #19263, #3530, #15617 ) ;
#14400 = CARTESIAN_POINT ( 'NONE',  ( -64.65223553951962288, 190.1463355405887228, 27.32593245744643795 ) ) ;
#14401 = ORIENTED_EDGE ( 'NONE', *, *, #4206, .F. ) ;
#14402 = CARTESIAN_POINT ( 'NONE',  ( 49.13077451860386446, 168.8134312302534283, 56.22586871687502708 ) ) ;
#14403 = DIRECTION ( 'NONE',  ( -1.386679829960243061E-14, 0.000000000000000000, -1.000000000000000000 ) ) ;
#14404 = ORIENTED_EDGE ( 'NONE', *, *, #6692, .T. ) ;
#14405 = FACE_OUTER_BOUND ( 'NONE', #65, .T. ) ;
#14406 = ORIENTED_EDGE ( 'NONE', *, *, #1103, .F. ) ;
#14407 = CARTESIAN_POINT ( 'NONE',  ( 64.99457118636310327, 169.9999999999999716, -0.8400692238016950197 ) ) ;
#14408 = CARTESIAN_POINT ( 'NONE',  ( 49.82165995907426037, 189.5987917270899459, -73.47870018378864643 ) ) ;
#14409 = CARTESIAN_POINT ( 'NONE',  ( -80.05923150692979107, 75.13699351169597662, -4.065642694558678549 ) ) ;
#14410 = CARTESIAN_POINT ( 'NONE',  ( -8.308020146049644339, 165.3460916013453641, 321.2202151032084316 ) ) ;
#14411 = CIRCLE ( 'NONE', #4462, 2.000000000000001332 ) ;
#14412 = AXIS2_PLACEMENT_3D ( 'NONE', #2736, #4765, #20396 ) ;
#14413 = AXIS2_PLACEMENT_3D ( 'NONE', #16919, #4603, #11630 ) ;
#14414 = CARTESIAN_POINT ( 'NONE',  ( 64.42259306105445660, 139.7551263635816952, -45.17031240767400391 ) ) ;
#14415 = PLANE ( 'NONE',  #19153 ) ;
#14416 = CARTESIAN_POINT ( 'NONE',  ( -8.792471272935635795, 81.92243737533797798, -84.90096239309919213 ) ) ;
#14417 = CARTESIAN_POINT ( 'NONE',  ( 41.20362701579343678, 107.2712125007551691, 92.86385812504968840 ) ) ;
#14418 = ORIENTED_EDGE ( 'NONE', *, *, #12599, .T. ) ;
#14419 = EDGE_CURVE ( 'NONE', #4965, #13170, #11433, .T. ) ;
#14420 = CIRCLE ( 'NONE', #14785, 87.00000000000001421 ) ;
#14421 = CARTESIAN_POINT ( 'NONE',  ( 41.19638261157623305, 121.2962013336460814, 247.0525242307099347 ) ) ;
#14422 = ORIENTED_EDGE ( 'NONE', *, *, #15708, .F. ) ;
#14423 = CARTESIAN_POINT ( 'NONE',  ( -105.2250167141420576, 70.47859713728956876, 32.05784361718416875 ) ) ;
#14424 = CARTESIAN_POINT ( 'NONE',  ( 19.80241179164982768, 183.7441055747629264, 315.5604959055339691 ) ) ;
#14425 = AXIS2_PLACEMENT_3D ( 'NONE', #11438, #2714, #7975 ) ;
#14426 = ORIENTED_EDGE ( 'NONE', *, *, #13747, .F. ) ;
#14427 = AXIS2_PLACEMENT_3D ( 'NONE', #9488, #15146, #6054 ) ;
#14428 = LINE ( 'NONE', #19104, #18305 ) ;
#14429 = CARTESIAN_POINT ( 'NONE',  ( 64.99457118636311748, 169.9999999999999716, -0.8400692238016952418 ) ) ;
#14430 = CARTESIAN_POINT ( 'NONE',  ( -6.705340559502253051, 144.4905701593873459, 277.0953757322560591 ) ) ;
#14431 = EDGE_CURVE ( 'NONE', #7715, #18203, #16503, .T. ) ;
#14432 = CARTESIAN_POINT ( 'NONE',  ( -90.71810225913505121, 79.29666913609149503, -27.07744225877266331 ) ) ;
#14433 = CARTESIAN_POINT ( 'NONE',  ( -49.64993871177497198, 140.1470898690141098, 27.40669857513504226 ) ) ;
#14434 = DIRECTION ( 'NONE',  ( 7.125109674161446091E-05, -0.9999848031710252272, 0.005512562950850307709 ) ) ;
#14435 = EDGE_CURVE ( 'NONE', #3953, #19042, #8259, .T. ) ;
#14436 = VECTOR ( 'NONE', #15522, 1000.000000000000000 ) ;
#14437 = DIRECTION ( 'NONE',  ( -1.387778780781445676E-14, 0.000000000000000000, 1.000000000000000000 ) ) ;
#14438 = PLANE ( 'NONE',  #16661 ) ;
#14439 = CARTESIAN_POINT ( 'NONE',  ( 12.90652684605866796, 190.4489680158945646, 307.8543765190132717 ) ) ;
#14440 = CARTESIAN_POINT ( 'NONE',  ( 83.95054225259531222, 104.7585062753441036, 71.08029813247935635 ) ) ;
#14441 = CARTESIAN_POINT ( 'NONE',  ( -51.82774057240565213, 118.9447701193097942, 172.1955447453271404 ) ) ;
#14442 =( LENGTH_UNIT ( ) NAMED_UNIT ( * ) SI_UNIT ( .MILLI., .METRE. ) );
#14443 =( BOUNDED_SURFACE ( )  B_SPLINE_SURFACE ( 3, 2, ( 
 ( #17300, #15587, #20176 ),
 ( #1560, #22000, #18584 ),
 ( #8546, #8652, #7904 ),
 ( #11473, #15695, #18479 ),
 ( #16876, #19231, #14941 ),
 ( #12123, #22535, #22636 ),
 ( #6827, #9754, #3385 ),
 ( #6301, #11588, #20830 ),
 ( #10401, #1678, #6933 ),
 ( #5211, #12244, #3500 ),
 ( #16663, #5666, #14439 ),
 ( #14546, #5325, #5434 ),
 ( #17883, #10515, #14206 ),
 ( #12467, #8888, #17640 ),
 ( #2225, #9002, #2115 ),
 ( #17527, #19779, #1780 ),
 ( #10617, #19455, #10961 ),
 ( #17987, #3604, #181 ),
 ( #21072, #9109, #3721 ),
 ( #14318, #12364, #21400 ),
 ( #1896, #8757, #21505 ),
 ( #21180, #21285, #15933 ),
 ( #9231, #12703, #15811 ),
 ( #7176, #10741, #5771 ),
 ( #19670, #7278, #16278 ),
 ( #17769, #19345, #3940 ),
 ( #55, #2013, #16048 ),
 ( #283, #5556, #7058 ),
 ( #12586, #19569, #3844 ),
 ( #10858, #16159, #518 ),
 ( #12806, #399, #7395 ),
 ( #14088, #7518, #7619 ),
 ( #21946, #19902, #4172 ),
 ( #18545, #18213, #20016 ),
 ( #4053, #13389, #11081 ),
 ( #11199, #6018, #4510 ),
 ( #11540, #2458, #16492 ),
 ( #14661, #2697, #21731 ),
 ( #7859, #5897, #7960 ),
 ( #9455, #18105, #15110 ),
 ( #2348, #746, #6368 ),
 ( #2802, #6243, #9349 ),
 ( #7741, #4279, #14994 ),
 ( #18431, #11304, #13269 ),
 ( #9810, #16826, #13055 ),
 ( #16726, #18308, #21612 ),
 ( #16387, #9706, #14781 ),
 ( #2575, #12933, #628 ),
 ( #9584, #16618, #869 ),
 ( #14896, #21838, #6128 ),
 ( #20247, #13154, #20118 ),
 ( #11418, #4389, #974 ),
 ( #1083, #22066, #8075 ),
 ( #17393, #22615, #17271 ),
 ( #15562, #1208, #6580 ),
 ( #3020, #8203, #2907 ) ),
 .UNSPECIFIED., .F., .F., .T. ) 
 B_SPLINE_SURFACE_WITH_KNOTS ( ( 4, 2, 2, 2, 2, 2, 2, 2, 2, 2, 2, 2, 2, 2, 2, 2, 2, 2, 2, 2, 2, 2, 2, 2, 2, 2, 2, 4 ),
 ( 3, 3 ),
 ( 0.1242173993009022120, 0.1244328327546842528, 0.1244866911181297664, 0.1245136202998525232, 0.1245405494815752800, 0.1246482662084663073, 0.1250791331160303888, 0.1259408669311585793, 0.1276643345614149605, 0.1293878021916713417, 0.1311112698219276951, 0.1328347374521840485, 0.1345582050824404297, 0.1362816727126968108, 0.1371434065278249737, 0.1380051403429531642, 0.1388668741580813548, 0.1397286079732095176, 0.1405903417883377082, 0.1414520756034658988, 0.1431755432337222800, 0.1440372770488504706, 0.1448990108639786611, 0.1457607446791068517, 0.1466224784942350423, 0.1483459461244913957, 0.1500694137547477491, 0.1517928813850041303 ),
 ( 0.000000000000000000, 1.000000000000000000 ),
 .UNSPECIFIED. ) 
 GEOMETRIC_REPRESENTATION_ITEM ( )  RATIONAL_B_SPLINE_SURFACE ( (
 ( 1.000000000000000000, 0.7202457815375945538, 1.000000000000000000),
 ( 1.000000000000000000, 0.7203148644494854480, 1.000000000000000000),
 ( 1.000000000000000000, 0.7203837616398036658, 1.000000000000000000),
 ( 1.000000000000000000, 0.7204696515171350457, 1.000000000000000000),
 ( 1.000000000000000000, 0.7204868179141954432, 1.000000000000000000),
 ( 1.000000000000000000, 0.7205125501470087679, 1.000000000000000000),
 ( 1.000000000000000000, 0.7205211246666077818, 1.000000000000000000),
 ( 1.000000000000000000, 0.7205382679145281299, 1.000000000000000000),
 ( 1.000000000000000000, 0.7207549634841317054, 1.000000000000000000),
 ( 1.000000000000000000, 0.7214802973574021561, 1.000000000000000000),
 ( 1.000000000000000000, 0.7220635808725176519, 1.000000000000000000),
 ( 1.000000000000000000, 0.7249944760233909546, 1.000000000000000000),
 ( 1.000000000000000000, 0.7273854792137299796, 1.000000000000000000),
 ( 1.000000000000000000, 0.7346752236034637118, 1.000000000000000000),
 ( 1.000000000000000000, 0.7396903655602768968, 1.000000000000000000),
 ( 1.000000000000000000, 0.7550399040982476162, 1.000000000000000000),
 ( 1.000000000000000000, 0.7655727772217874039, 1.000000000000000000),
 ( 1.000000000000000000, 0.7871107331848644639, 1.000000000000000000),
 ( 1.000000000000000000, 0.7981416010053231647, 1.000000000000000000),
 ( 1.000000000000000000, 0.8197093954368291913, 1.000000000000000000),
 ( 1.000000000000000000, 0.8303367115343781579, 1.000000000000000000),
 ( 1.000000000000000000, 0.8510544108449787926, 1.000000000000000000),
 ( 1.000000000000000000, 0.8611795848883848636, 1.000000000000000000),
 ( 1.000000000000000000, 0.8805664355309501534, 1.000000000000000000),
 ( 1.000000000000000000, 0.8897650402490725474, 1.000000000000000000),
 ( 1.000000000000000000, 0.9068567199018958691, 1.000000000000000000),
 ( 1.000000000000000000, 0.9147565445290845032, 1.000000000000000000),
 ( 1.000000000000000000, 0.9255566967665967981, 1.000000000000000000),
 ( 1.000000000000000000, 0.9289711410761075649, 1.000000000000000000),
 ( 1.000000000000000000, 0.9352102042489658373, 1.000000000000000000),
 ( 1.000000000000000000, 0.9380652775089347584, 1.000000000000000000),
 ( 1.000000000000000000, 0.9432152439419067003, 1.000000000000000000),
 ( 1.000000000000000000, 0.9455148386610635614, 1.000000000000000000),
 ( 1.000000000000000000, 0.9494488520115715868, 1.000000000000000000),
 ( 1.000000000000000000, 0.9510350116254054909, 1.000000000000000000),
 ( 1.000000000000000000, 0.9534119305046732107, 1.000000000000000000),
 ( 1.000000000000000000, 0.9542080638533945169, 1.000000000000000000),
 ( 1.000000000000000000, 0.9549528115835310693, 1.000000000000000000),
 ( 1.000000000000000000, 0.9548852033311120424, 1.000000000000000000),
 ( 1.000000000000000000, 0.9533785252478389483, 1.000000000000000000),
 ( 1.000000000000000000, 0.9507260831990033134, 1.000000000000000000),
 ( 1.000000000000000000, 0.9445325143455129968, 1.000000000000000000),
 ( 1.000000000000000000, 0.9421267862709985508, 1.000000000000000000),
 ( 1.000000000000000000, 0.9368091832047875656, 1.000000000000000000),
 ( 1.000000000000000000, 0.9338841920341318659, 1.000000000000000000),
 ( 1.000000000000000000, 0.9275336217117351456, 1.000000000000000000),
 ( 1.000000000000000000, 0.9240930730323024811, 1.000000000000000000),
 ( 1.000000000000000000, 0.9167918297806771921, 1.000000000000000000),
 ( 1.000000000000000000, 0.9129208614828339119, 1.000000000000000000),
 ( 1.000000000000000000, 0.9008886848957327054, 1.000000000000000000),
 ( 1.000000000000000000, 0.8922078542948799207, 1.000000000000000000),
 ( 1.000000000000000000, 0.8738477936028254955, 1.000000000000000000),
 ( 1.000000000000000000, 0.8641886109620656731, 1.000000000000000000),
 ( 1.000000000000000000, 0.8438841653332657122, 1.000000000000000000),
 ( 1.000000000000000000, 0.8333285471625734298, 1.000000000000000000),
 ( 1.000000000000000000, 0.8227386401547407413, 1.000000000000000000) ) ) 
 REPRESENTATION_ITEM ( '' )  SURFACE ( )  );
#14444 = AXIS2_PLACEMENT_3D ( 'NONE', #8002, #4441, #2403 ) ;
#14445 = CIRCLE ( 'NONE', #15547, 112.5000000000000142 ) ;
#14446 = ADVANCED_FACE ( 'NONE', ( #2814 ), #16839, .T. ) ;
#14447 = DIRECTION ( 'NONE',  ( 0.009138748381789078140, -0.7071067811865487940, 0.7070477234798315802 ) ) ;
#14448 = FACE_OUTER_BOUND ( 'NONE', #10392, .T. ) ;
#14449 = ADVANCED_FACE ( 'NONE', ( #16397 ), #15311, .F. ) ;
#14450 = EDGE_LOOP ( 'NONE', ( #17872, #21750 ) ) ;
#14451 = CARTESIAN_POINT ( 'NONE',  ( -93.21002351426730570, 79.82103140525721585, -28.79774562292282170 ) ) ;
#14452 = ORIENTED_EDGE ( 'NONE', *, *, #13184, .T. ) ;
#14453 = EDGE_CURVE ( 'NONE', #5372, #22420, #10052, .T. ) ;
#14454 = CARTESIAN_POINT ( 'NONE',  ( -0.8801090646609086576, 70.01899995639456620, -99.03135606234927479 ) ) ;
#14455 = CARTESIAN_POINT ( 'NONE',  ( 23.17824588921087781, -5.346239964818104262, -10.63114771928880309 ) ) ;
#14456 = CARTESIAN_POINT ( 'NONE',  ( -10.85595612533484911, 109.6999345499266525, 127.2773526115149281 ) ) ;
#14457 = AXIS2_PLACEMENT_3D ( 'NONE', #11560, #9828, #16846 ) ;
#14458 = CARTESIAN_POINT ( 'NONE',  ( 68.30941429790007646, 191.4143309225247549, 255.6230893828509352 ) ) ;
#14459 = AXIS2_PLACEMENT_3D ( 'NONE', #3713, #17523, #20825 ) ;
#14460 = CARTESIAN_POINT ( 'NONE',  ( -164.0000000000000000, 1.999999999999998224, 53.76161406891260697 ) ) ;
#14461 = ADVANCED_FACE ( 'NONE', ( #1667 ), #21446, .F. ) ;
#14462 = EDGE_LOOP ( 'NONE', ( #14626, #13121, #22506, #17935 ) ) ;
#14463 = DIRECTION ( 'NONE',  ( 0.9232306267972772984, 1.069144893909150629E-19, -0.3842462878721229491 ) ) ;
#14464 = ORIENTED_EDGE ( 'NONE', *, *, #4591, .T. ) ;
#14465 = DIRECTION ( 'NONE',  ( 0.9999164797902015955, 0.000000000000000000, -0.01292414190463697134 ) ) ;
#14466 = EDGE_CURVE ( 'NONE', #15997, #2837, #22524, .T. ) ;
#14467 = DIRECTION ( 'NONE',  ( 7.125109674161246868E-05, -0.9999848031710252272, 0.005512562950850154186 ) ) ;
#14468 = CARTESIAN_POINT ( 'NONE',  ( 52.91240873130399081, 106.8060942374655156, 70.25530070199208410 ) ) ;
#14469 = FACE_OUTER_BOUND ( 'NONE', #14350, .T. ) ;
#14470 = FACE_OUTER_BOUND ( 'NONE', #9493, .T. ) ;
#14471 = VECTOR ( 'NONE', #10218, 999.9999999999998863 ) ;
#14472 = AXIS2_PLACEMENT_3D ( 'NONE', #20117, #16616, #7959 ) ;
#14473 = VERTEX_POINT ( 'NONE', #6710 ) ;
#14474 = LINE ( 'NONE', #21438, #14003 ) ;
#14475 = ORIENTED_EDGE ( 'NONE', *, *, #6493, .T. ) ;
#14476 = DIRECTION ( 'NONE',  ( 0.9999164797902015955, 2.001050586450178695E-22, -0.01292414190464131335 ) ) ;
#14477 = CARTESIAN_POINT ( 'NONE',  ( -15.55314327042932376, 177.7443265726918469, 314.9881042928857369 ) ) ;
#14478 = VERTEX_POINT ( 'NONE', #12000 ) ;
#14479 = EDGE_CURVE ( 'NONE', #16185, #14111, #3373, .T. ) ;
#14480 = CONICAL_SURFACE ( 'NONE', #21050, 9.000000000000001776, 1.047197551196594301 ) ;
#14481 = CIRCLE ( 'NONE', #18488, 10.29357798165139393 ) ;
#14482 = DIRECTION ( 'NONE',  ( -0.01292394549866739996, -0.005513023399721118760, -0.9999012842304692006 ) ) ;
#14483 = EDGE_CURVE ( 'NONE', #9660, #2844, #534, .T. ) ;
#14484 = ORIENTED_EDGE ( 'NONE', *, *, #798, .T. ) ;
#14485 = LINE ( 'NONE', #5710, #10730 ) ;
#14486 = VECTOR ( 'NONE', #17130, 999.9999999999998863 ) ;
#14487 = CARTESIAN_POINT ( 'NONE',  ( -37.83293359760840247, 93.41702043942370892, 84.07896005544418472 ) ) ;
#14488 = DIRECTION ( 'NONE',  ( 0.9999164797902015955, 2.001050586450178695E-22, -0.01292414190464131335 ) ) ;
#14489 = EDGE_CURVE ( 'NONE', #9463, #4261, #3092, .T. ) ;
#14490 = DIRECTION ( 'NONE',  ( 0.009760756503428048153, -0.9999378516499565217, 0.005387065077612505741 ) ) ;
#14491 = AXIS2_PLACEMENT_3D ( 'NONE', #19927, #16852, #8110 ) ;
#14492 = VERTEX_POINT ( 'NONE', #8313 ) ;
#14493 = CIRCLE ( 'NONE', #21053, 2.499999999999988010 ) ;
#14494 = CARTESIAN_POINT ( 'NONE',  ( -0.003538370294055813436, 69.99999999999998579, -98.91746206376724615 ) ) ;
#14495 = CARTESIAN_POINT ( 'NONE',  ( -8.312614011469616315, 69.99999999999998579, -95.45924547291811280 ) ) ;
#14496 = ORIENTED_EDGE ( 'NONE', *, *, #19194, .T. ) ;
#14497 = CARTESIAN_POINT ( 'NONE',  ( -4.153117824915283585, 189.6079574532614060, 275.5417844139159911 ) ) ;
#14498 = CARTESIAN_POINT ( 'NONE',  ( -105.4334892372614121, 72.00000000000000000, 31.36525700924958926 ) ) ;
#14499 = CARTESIAN_POINT ( 'NONE',  ( -40.55508067841016384, 96.01222808543204223, -41.81663866985299194 ) ) ;
#14500 = ORIENTED_EDGE ( 'NONE', *, *, #27, .T. ) ;
#14501 = CARTESIAN_POINT ( 'NONE',  ( 18.53667494532311721, 147.4324440254954993, 278.1633530095816127 ) ) ;
#14502 = LINE ( 'NONE', #2642, #6593 ) ;
#14503 = ADVANCED_FACE ( 'NONE', ( #22417 ), #14120, .F. ) ;
#14504 = EDGE_CURVE ( 'NONE', #13316, #10917, #8535, .T. ) ;
#14505 = ORIENTED_EDGE ( 'NONE', *, *, #12257, .T. ) ;
#14506 = CIRCLE ( 'NONE', #7513, 10.00000000000000711 ) ;
#14507 = DIRECTION ( 'NONE',  ( 7.125109674160258889E-05, -0.9999848031710252272, 0.005512562950849897447 ) ) ;
#14508 = CARTESIAN_POINT ( 'NONE',  ( -146.5000000000000000, 1.999999999999998224, 2.081668171172168513E-14 ) ) ;
#14509 = APPLICATION_PROTOCOL_DEFINITION ( 'draft international standard', 'automotive_design', 1998, #7783 ) ;
#14510 = ORIENTED_EDGE ( 'NONE', *, *, #8479, .F. ) ;
#14511 = EDGE_LOOP ( 'NONE', ( #5160, #9443, #3372 ) ) ;
#14512 = DIRECTION ( 'NONE',  ( -0.9999164797902017066, -6.965998958219367529E-18, 0.01292414190464157182 ) ) ;
#14513 = DIRECTION ( 'NONE',  ( 7.125109674364536131E-05, -0.9999848031710253382, 0.005512562950849705760 ) ) ;
#14514 = VERTEX_POINT ( 'NONE', #5080 ) ;
#14515 = DIRECTION ( 'NONE',  ( -0.9999164797902017066, -2.001050586450178931E-22, 0.01292414190464131508 ) ) ;
#14516 = CARTESIAN_POINT ( 'NONE',  ( -90.75111155332035651, 98.75957274858885171, -62.16377225325074818 ) ) ;
#14517 = EDGE_LOOP ( 'NONE', ( #241, #3504, #2057, #2998 ) ) ;
#14518 = DIRECTION ( 'NONE',  ( 0.7069973413461587697, 0.7070960354057281849, -0.01303671902605484795 ) ) ;
#14519 = ORIENTED_EDGE ( 'NONE', *, *, #4272, .F. ) ;
#14520 = CARTESIAN_POINT ( 'NONE',  ( -12.81536461602102683, 326.2504838843369726, 414.3222871145668478 ) ) ;
#14521 = CARTESIAN_POINT ( 'NONE',  ( 49.44092383899086229, 189.5967114759612286, -73.85113886024416274 ) ) ;
#14522 = CARTESIAN_POINT ( 'NONE',  ( -2.752290252500367629, 142.9573650401683267, 275.1042456662929681 ) ) ;
#14523 = CARTESIAN_POINT ( 'NONE',  ( -22.57586261656929238, 324.7034503240921026, 307.5610645536022503 ) ) ;
#14524 = FACE_BOUND ( 'NONE', #118, .T. ) ;
#14525 = DIRECTION ( 'NONE',  ( -2.025474946048326158E-22, 1.000000000000000000, -1.876735158486679638E-22 ) ) ;
#14526 = DIRECTION ( 'NONE',  ( -0.01292394549866695240, -0.005513023399718316314, -0.9999012842304693116 ) ) ;
#14527 = DIRECTION ( 'NONE',  ( 0.000000000000000000, 0.000000000000000000, -1.000000000000000000 ) ) ;
#14528 = ORIENTED_EDGE ( 'NONE', *, *, #15872, .F. ) ;
#14529 = ADVANCED_FACE ( 'NONE', ( #17073 ), #12113, .F. ) ;
#14530 = FACE_BOUND ( 'NONE', #3582, .T. ) ;
#14531 = FACE_OUTER_BOUND ( 'NONE', #11601, .T. ) ;
#14532 = ORIENTED_EDGE ( 'NONE', *, *, #15684, .T. ) ;
#14533 = VECTOR ( 'NONE', #16343, 1000.000000000000000 ) ;
#14534 = CARTESIAN_POINT ( 'NONE',  ( -84.80959639660540006, 75.01379216013428675, 2.744183072880618468 ) ) ;
#14535 = CARTESIAN_POINT ( 'NONE',  ( 19.56521222682726702, 184.0192530622549043, 312.4160503478434521 ) ) ;
#14537 = ORIENTED_EDGE ( 'NONE', *, *, #4996, .F. ) ;
#14536 = ORIENTED_EDGE ( 'NONE', *, *, #12120, .T. ) ;
#14538 = FACE_OUTER_BOUND ( 'NONE', #18829, .T. ) ;
#14539 = DIRECTION ( 'NONE',  ( 0.9999164797902015955, 6.965998958219364448E-18, -0.01292414190464157182 ) ) ;
#14540 = CARTESIAN_POINT ( 'NONE',  ( -91.00106904273528130, 70.29040131071506892, 61.79648398638329354 ) ) ;
#14541 = DIRECTION ( 'NONE',  ( -0.9999164797902015955, -2.219203356785933794E-15, 0.01292414190464157009 ) ) ;
#14542 = VERTEX_POINT ( 'NONE', #15246 ) ;
#14543 = CARTESIAN_POINT ( 'NONE',  ( -10.03308090247307405, 188.0016273849522861, 308.1595840160059083 ) ) ;
#14544 = AXIS2_PLACEMENT_3D ( 'NONE', #11486, #11362, #2640 ) ;
#14545 = CARTESIAN_POINT ( 'NONE',  ( 73.73856782067191773, 74.99999999999998579, -1.361083785117223499 ) ) ;
#14546 = CARTESIAN_POINT ( 'NONE',  ( 12.19776044723496256, 187.6128494603106276, 304.9050912290015276 ) ) ;
#14547 = CARTESIAN_POINT ( 'NONE',  ( 91.87497954589152016, 77.44324451750787830, 29.32612497091767878 ) ) ;
#14548 = FACE_OUTER_BOUND ( 'NONE', #16169, .T. ) ;
#14549 = ORIENTED_EDGE ( 'NONE', *, *, #4177, .T. ) ;
#14550 = CARTESIAN_POINT ( 'NONE',  ( -93.23587179807654479, 72.00000000000000000, -30.79757858250321689 ) ) ;
#14551 = LINE ( 'NONE', #4285, #22382 ) ;
#14552 = ORIENTED_EDGE ( 'NONE', *, *, #17952, .T. ) ;
#14553 = DIRECTION ( 'NONE',  ( 0.1337561903331544733, 0.9909881666746205298, -0.007192708699472569189 ) ) ;
#14554 = ORIENTED_EDGE ( 'NONE', *, *, #853, .T. ) ;
#14555 = ADVANCED_FACE ( 'NONE', ( #6922 ), #11661, .T. ) ;
#14556 = ORIENTED_EDGE ( 'NONE', *, *, #4557, .F. ) ;
#14557 = B_SPLINE_CURVE_WITH_KNOTS ( 'NONE', 3,
 ( #14200, #21174, #16041, #3838, #278, #5427 ),
 .UNSPECIFIED., .F., .F.,
 ( 4, 2, 4 ),
 ( 0.001327491350857572250, 0.002295428894073542163, 0.003263366437289511642 ),
 .UNSPECIFIED. ) ;
#14558 = DIRECTION ( 'NONE',  ( -0.01292394549866744159, -0.005513023399721009472, -0.9999012842304692006 ) ) ;
#14559 = EDGE_CURVE ( 'NONE', #7441, #8239, #1283, .T. ) ;
#14560 = DIRECTION ( 'NONE',  ( 0.01292394549866733404, 0.005513023399720420534, 0.9999012842304693116 ) ) ;
#14561 = CARTESIAN_POINT ( 'NONE',  ( 74.93593926291724472, 75.00181558815791050, -0.2967849484207667476 ) ) ;
#14562 = CARTESIAN_POINT ( 'NONE',  ( -41.00865927789263310, 166.2639521169525665, 308.9298270502609967 ) ) ;
#14563 = ORIENTED_EDGE ( 'NONE', *, *, #20735, .F. ) ;
#14564 = DIRECTION ( 'NONE',  ( 0.01292394549866733230, 0.005513023399720419666, 0.9999012842304692006 ) ) ;
#14565 = DIRECTION ( 'NONE',  ( 0.000000000000000000, 0.000000000000000000, 1.000000000000000000 ) ) ;
#14566 = EDGE_CURVE ( 'NONE', #22043, #2491, #6490, .T. ) ;
#14567 = CARTESIAN_POINT ( 'NONE',  ( 163.9999999999998863, 0.8284271247461897358, 8.000000000002229328 ) ) ;
#14568 = B_SPLINE_CURVE_WITH_KNOTS ( 'NONE', 3,
 ( #22445, #17662, #10416, #6734, #2024, #13757 ),
 .UNSPECIFIED., .F., .F.,
 ( 4, 2, 4 ),
 ( 2.380730968223736687E-07, 0.002629065763328342683, 0.005257893453559862873 ),
 .UNSPECIFIED. ) ;
#14569 =( BOUNDED_SURFACE ( )  B_SPLINE_SURFACE ( 3, 2, ( 
 ( #19259, #19481, #3631 ),
 ( #1805, #3756, #12497 ),
 ( #10769, #3525, #20979 ),
 ( #5232, #7429, #10879 ),
 ( #8790, #2139, #12275 ),
 ( #15844, #9139, #16191 ),
 ( #14230, #431, #10537 ),
 ( #313, #21434, #8914 ),
 ( #7305, #87, #5696 ),
 ( #14115, #10644, #17679 ),
 ( #1927, #203, #15964 ),
 ( #21204, #11568, #9738 ),
 ( #11449, #9617, #5926 ),
 ( #15026, #4081, #6161 ),
 ( #7548, #11228, #7886 ),
 ( #7642, #20048, #13186 ),
 ( #16647, #658, #4305 ),
 ( #19930, #20152, #14576 ) ),
 .UNSPECIFIED., .F., .F., .T. ) 
 B_SPLINE_SURFACE_WITH_KNOTS ( ( 4, 2, 2, 2, 2, 2, 2, 2, 4 ),
 ( 3, 3 ),
 ( 0.08392082777186243847, 0.08669808355430655422, 0.08808671144552862597, 0.08878102539113966185, 0.08912818236394517979, 0.08930176085034793876, 0.08934515547194862850, 0.08938855009354931824, 0.08947533933675068385 ),
 ( 0.000000000000000000, 1.000000000000000000 ),
 .UNSPECIFIED. ) 
 GEOMETRIC_REPRESENTATION_ITEM ( )  RATIONAL_B_SPLINE_SURFACE ( (
 ( 1.000000000000000000, 0.8227386401548728578, 1.000000000000000000),
 ( 1.000000000000000000, 0.8263415838687132586, 1.000000000000000000),
 ( 1.000000000000000000, 0.8288608359724080055, 1.000000000000000000),
 ( 1.000000000000000000, 0.8282189721166841601, 1.000000000000000000),
 ( 1.000000000000000000, 0.8271574078635184346, 1.000000000000000000),
 ( 1.000000000000000000, 0.8239197622700882295, 1.000000000000000000),
 ( 1.000000000000000000, 0.8225730560414692416, 1.000000000000000000),
 ( 1.000000000000000000, 0.8201245374459615878, 1.000000000000000000),
 ( 1.000000000000000000, 0.8192370252863434565, 1.000000000000000000),
 ( 1.000000000000000000, 0.8177961922883111301, 1.000000000000000000),
 ( 1.000000000000000000, 0.8172976608660983411, 1.000000000000000000),
 ( 1.000000000000000000, 0.8166514735310177464, 1.000000000000000000),
 ( 1.000000000000000000, 0.8167936669037794140, 1.000000000000000000),
 ( 1.000000000000000000, 0.8168953424636213878, 1.000000000000000000),
 ( 1.000000000000000000, 0.8169461963287523165, 1.000000000000000000),
 ( 1.000000000000000000, 0.8170988061681787595, 1.000000000000000000),
 ( 1.000000000000000000, 0.8172006103753840511, 1.000000000000000000),
 ( 1.000000000000000000, 0.8173024788409735120, 1.000000000000000000) ) ) 
 REPRESENTATION_ITEM ( '' )  SURFACE ( )  );
#14570 = ORIENTED_EDGE ( 'NONE', *, *, #19388, .T. ) ;
#14571 = CARTESIAN_POINT ( 'NONE',  ( -68.71681667565952978, 91.17157287525388654, 85.89527988174785378 ) ) ;
#14572 = DIRECTION ( 'NONE',  ( 0.9784407279240388000, -0.001140033730246431398, -0.2065246771273868409 ) ) ;
#14573 = LINE ( 'NONE', #2383, #22491 ) ;
#14574 = EDGE_CURVE ( 'NONE', #22174, #8492, #5541, .T. ) ;
#14575 = CARTESIAN_POINT ( 'NONE',  ( 68.50871000753478768, 71.18193548034264495, -86.06142760398537916 ) ) ;
#14576 = CARTESIAN_POINT ( 'NONE',  ( -8.305185890944088101, 185.3905336583419512, 323.2540923045081058 ) ) ;
#14577 = CARTESIAN_POINT ( 'NONE',  ( -89.76942472236369497, 79.35227432041517659, 29.58847612530658111 ) ) ;
#14578 = CARTESIAN_POINT ( 'NONE',  ( -162.0000000000000000, 20.00000000000000000, -9.999999999999978684 ) ) ;
#14579 = ORIENTED_EDGE ( 'NONE', *, *, #10497, .F. ) ;
#14580 = CARTESIAN_POINT ( 'NONE',  ( -12.58664483627419095, 184.6272112293399630, 320.1917372557430213 ) ) ;
#14581 = PLANE ( 'NONE',  #8436 ) ;
#14582 = CARTESIAN_POINT ( 'NONE',  ( -14.97537071516516427, 178.7788208869449136, 313.2939786621885787 ) ) ;
#14583 = ORIENTED_EDGE ( 'NONE', *, *, #11899, .F. ) ;
#14584 = EDGE_CURVE ( 'NONE', #22007, #5091, #12281, .T. ) ;
#14585 = EDGE_LOOP ( 'NONE', ( #21251, #15605 ) ) ;
#14586 = DIRECTION ( 'NONE',  ( 0.01292414190464174703, 0.000000000000000000, 0.9999164797902015955 ) ) ;
#14587 = EDGE_CURVE ( 'NONE', #20005, #126, #16708, .T. ) ;
#14588 = EDGE_CURVE ( 'NONE', #4299, #18381, #5656, .T. ) ;
#14589 = ADVANCED_FACE ( 'NONE', ( #9215, #12570 ), #17871, .F. ) ;
#14590 = ORIENTED_EDGE ( 'NONE', *, *, #541, .T. ) ;
#14591 = EDGE_CURVE ( 'NONE', #10233, #21383, #4919, .T. ) ;
#14592 = DIRECTION ( 'NONE',  ( -0.000000000000000000, -1.000000000000000000, -0.000000000000000000 ) ) ;
#14593 = CARTESIAN_POINT ( 'NONE',  ( -34.61804907780420137, 94.93197183469658285, 82.52232902628021805 ) ) ;
#14594 = CARTESIAN_POINT ( 'NONE',  ( -10.85795115604361349, 137.6995090387153482, 127.1230008488911096 ) ) ;
#14595 = CARTESIAN_POINT ( 'NONE',  ( 49.39754356754257714, 108.7350236001487502, -46.93403478043238408 ) ) ;
#14596 = EDGE_LOOP ( 'NONE', ( #6921, #20798, #13730 ) ) ;
#14597 = DIRECTION ( 'NONE',  ( -0.01292394549866738608, -0.005513023399720699824, -0.9999012842304692006 ) ) ;
#14598 = EDGE_LOOP ( 'NONE', ( #21300, #7949, #14166, #10170 ) ) ;
#14599 = EDGE_CURVE ( 'NONE', #2340, #3568, #7873, .T. ) ;
#14600 = DIRECTION ( 'NONE',  ( 0.009188991635466050092, -0.7031977391749439921, 0.7109349492407662785 ) ) ;
#14601 = ORIENTED_EDGE ( 'NONE', *, *, #18755, .T. ) ;
#14602 = ORIENTED_EDGE ( 'NONE', *, *, #13562, .T. ) ;
#14603 = CARTESIAN_POINT ( 'NONE',  ( -71.30561357180762627, 88.42313952667566923, 69.70915026362466449 ) ) ;
#14604 = ORIENTED_EDGE ( 'NONE', *, *, #21469, .T. ) ;
#14605 = CARTESIAN_POINT ( 'NONE',  ( 12.53551711061738594, 188.9428922227077976, 321.3016085981989818 ) ) ;
#14606 = PLANE ( 'NONE',  #12417 ) ;
#14607 = CARTESIAN_POINT ( 'NONE',  ( 0.2091060127835376314, 86.14731717667953603, 75.00341234062101137 ) ) ;
#14608 = DIRECTION ( 'NONE',  ( 0.01292394549866738782, 0.005513023399720700692, 0.9999012842304693116 ) ) ;
#14609 = CIRCLE ( 'NONE', #6861, 1.999999999999998446 ) ;
#14610 = EDGE_CURVE ( 'NONE', #14478, #11658, #14134, .T. ) ;
#14611 = ORIENTED_EDGE ( 'NONE', *, *, #2641, .F. ) ;
#14612 = CARTESIAN_POINT ( 'NONE',  ( -91.62437796271721879, 34.61572286322119396, -60.86849236629028326 ) ) ;
#14613 = CARTESIAN_POINT ( 'NONE',  ( -89.27750275332233798, 88.44712234866830158, 50.50536220203945703 ) ) ;
#14614 = CARTESIAN_POINT ( 'NONE',  ( -205.7907554531092273, 125.4195586025777516, 299.0696188052555726 ) ) ;
#14616 = ORIENTED_EDGE ( 'NONE', *, *, #12095, .F. ) ;
#14615 = VERTEX_POINT ( 'NONE', #3706 ) ;
#14617 = CARTESIAN_POINT ( 'NONE',  ( 36.55288090549195346, 94.02752048664900997, -83.45186405039071076 ) ) ;
#14618 = DIRECTION ( 'NONE',  ( 1.000000000000000000, -0.000000000000000000, -9.912705577010318154E-17 ) ) ;
#14619 = VERTEX_POINT ( 'NONE', #17973 ) ;
#14620 = DIRECTION ( 'NONE',  ( -0.7944560844389304544, 0.000000000000000000, -0.6073216033519334145 ) ) ;
#14621 = LINE ( 'NONE', #21576, #3401 ) ;
#14622 = DIRECTION ( 'NONE',  ( -0.9770372205688159228, 0.2127605332646583802, 0.01145535281434409414 ) ) ;
#14623 = CARTESIAN_POINT ( 'NONE',  ( -39.75021781620441885, 69.99999999999998579, -86.03367798009510636 ) ) ;
#14624 = CIRCLE ( 'NONE', #19349, 4.399999999999996803 ) ;
#14625 = CARTESIAN_POINT ( 'NONE',  ( -91.26258897903520051, 97.45270810253440175, -61.41003422490167196 ) ) ;
#14626 = ORIENTED_EDGE ( 'NONE', *, *, #22479, .F. ) ;
#14627 = EDGE_CURVE ( 'NONE', #17067, #19550, #15117, .T. ) ;
#14628 = DIRECTION ( 'NONE',  ( 7.125109674364534776E-05, -0.9999848031710252272, 0.005512562950849704893 ) ) ;
#14629 = ORIENTED_EDGE ( 'NONE', *, *, #9209, .T. ) ;
#14630 = CARTESIAN_POINT ( 'NONE',  ( -109.6363981638670566, 79.04398536104964990, 28.84204567386064255 ) ) ;
#14631 = CARTESIAN_POINT ( 'NONE',  ( -92.13597290369312987, 77.31823782845361848, -29.12178019517726213 ) ) ;
#14632 = DIRECTION ( 'NONE',  ( 7.125109674364534776E-05, -0.9999848031710252272, 0.005512562950849704893 ) ) ;
#14633 = CARTESIAN_POINT ( 'NONE',  ( -11.14411950718743682, 70.55988472974013348, -90.55128027993727358 ) ) ;
#14634 = CARTESIAN_POINT ( 'NONE',  ( 59.65144567478507298, 126.9191314136042479, 166.0817088952479139 ) ) ;
#14635 = EDGE_LOOP ( 'NONE', ( #20281, #22184, #1826, #19140 ) ) ;
#14636 = FACE_OUTER_BOUND ( 'NONE', #1751, .T. ) ;
#14637 = CARTESIAN_POINT ( 'NONE',  ( -8.125559787506114517, 81.64068272718454011, -83.29857057268343112 ) ) ;
#14638 = DIRECTION ( 'NONE',  ( -0.01292394549866632963, -0.005513023399716958026, -0.9999012842304692006 ) ) ;
#14639 = AXIS2_PLACEMENT_3D ( 'NONE', #19578, #5674, #16055 ) ;
#14640 = ORIENTED_EDGE ( 'NONE', *, *, #8301, .T. ) ;
#14641 = CARTESIAN_POINT ( 'NONE',  ( 12.84375058515307089, 190.4863273772031960, 307.8501935766865927 ) ) ;
#14642 = ORIENTED_EDGE ( 'NONE', *, *, #5685, .T. ) ;
#14643 = EDGE_LOOP ( 'NONE', ( #14874, #18238, #454 ) ) ;
#14644 = B_SPLINE_CURVE_WITH_KNOTS ( 'NONE', 3,
 ( #17250, #7013, #19300, #11975, #14042, #21027, #3563, #21355 ),
 .UNSPECIFIED., .F., .F.,
 ( 4, 2, 2, 4 ),
 ( 0.005257893453559989508, 0.006567392922673304101, 0.007876892391786620429, 0.01049589133001324961 ),
 .UNSPECIFIED. ) ;
#14645 = CARTESIAN_POINT ( 'NONE',  ( -85.08821190676783885, 75.00001493645879691, 1.440439948039162088 ) ) ;
#14646 = CARTESIAN_POINT ( 'NONE',  ( 13.21943290499836543, 190.2582281869503049, 307.8807104300166202 ) ) ;
#14648 = ORIENTED_EDGE ( 'NONE', *, *, #16007, .T. ) ;
#14647 = ORIENTED_EDGE ( 'NONE', *, *, #11319, .T. ) ;
#14649 = VERTEX_POINT ( 'NONE', #14764 ) ;
#14650 = CARTESIAN_POINT ( 'NONE',  ( 40.75315251118328774, 108.3652131041115467, 58.01149545304486566 ) ) ;
#14651 = CARTESIAN_POINT ( 'NONE',  ( 40.73863394693862006, 95.06543039568907716, -44.50011052238011189 ) ) ;
#14652 = CARTESIAN_POINT ( 'NONE',  ( -41.61793149762837629, 72.00000000000000000, -86.46934588545651934 ) ) ;
#14653 = CIRCLE ( 'NONE', #3615, 87.00000000000001421 ) ;
#14654 = CARTESIAN_POINT ( 'NONE',  ( -89.99332827844999372, 79.52815953299852936, -27.82019389467126658 ) ) ;
#14655 = CARTESIAN_POINT ( 'NONE',  ( 70.22615711568096231, 70.59893530615325119, 84.66585046671892201 ) ) ;
#14656 = ADVANCED_FACE ( 'NONE', ( #4041 ), #2809, .T. ) ;
#14657 = ADVANCED_FACE ( 'NONE', ( #11493 ), #13404, .T. ) ;
#14658 = VECTOR ( 'NONE', #132, 999.9999999999998863 ) ;
#14659 = DIRECTION ( 'NONE',  ( 7.125109674403837105E-05, -0.9999848031710252272, 0.005512562950847867821 ) ) ;
#14660 = CARTESIAN_POINT ( 'NONE',  ( 79.99331838321626265, 55.99999999999999289, -7.033931352371318724 ) ) ;
#14661 = CARTESIAN_POINT ( 'NONE',  ( 20.69718713607370475, 181.8844827137008053, 314.2148154440831718 ) ) ;
#14662 = CARTESIAN_POINT ( 'NONE',  ( 93.13093775432295729, 79.82103140525535423, 28.79876782389523271 ) ) ;
#14663 = CYLINDRICAL_SURFACE ( 'NONE', #15069, 4.000000000000006217 ) ;
#14664 =( NAMED_UNIT ( * ) SI_UNIT ( $, .STERADIAN. ) SOLID_ANGLE_UNIT ( ) );
#14665 = CARTESIAN_POINT ( 'NONE',  ( -49.09967157776827662, 108.0238286078847523, 69.97982874036236467 ) ) ;
#14666 = CYLINDRICAL_SURFACE ( 'NONE', #9586, 2.000000000000004885 ) ;
#14667 = ORIENTED_EDGE ( 'NONE', *, *, #7101, .T. ) ;
#14668 = DIRECTION ( 'NONE',  ( -5.440186201345738641E-18, -1.000000000000000000, -1.334940939666364181E-17 ) ) ;
#14669 = AXIS2_PLACEMENT_3D ( 'NONE', #12579, #7272, #17982 ) ;
#14670 = ORIENTED_EDGE ( 'NONE', *, *, #6988, .F. ) ;
#14671 = CARTESIAN_POINT ( 'NONE',  ( -26.94222022802838268, 95.51270090492251086, 82.01937116434973518 ) ) ;
#14672 = AXIS2_PLACEMENT_3D ( 'NONE', #12534, #10919, #16230 ) ;
#14673 = CARTESIAN_POINT ( 'NONE',  ( -58.84901841222320229, 118.8937358571614453, 163.0286266904498405 ) ) ;
#14674 = CARTESIAN_POINT ( 'NONE',  ( 78.41260081656773195, 75.12325561942539309, 3.826278609843483114 ) ) ;
#14675 = CARTESIAN_POINT ( 'NONE',  ( 49.99582398951009310, 170.0000000000008242, -0.6462070952312342076 ) ) ;
#14676 = ORIENTED_EDGE ( 'NONE', *, *, #16007, .F. ) ;
#14677 = LINE ( 'NONE', #11102, #6689 ) ;
#14678 = CARTESIAN_POINT ( 'NONE',  ( 73.74384038452764401, 74.99999999999998579, -0.9531554654672949045 ) ) ;
#14679 = DIRECTION ( 'NONE',  ( -0.01292414190463827932, 0.000000000000000000, -0.9999164797902018176 ) ) ;
#14680 = VERTEX_POINT ( 'NONE', #7919 ) ;
#14681 = DIRECTION ( 'NONE',  ( 2.025474946048326158E-22, -1.000000000000000000, 1.876735158486679638E-22 ) ) ;
#14682 = DIRECTION ( 'NONE',  ( 1.000000000000000000, 0.000000000000000000, 0.000000000000000000 ) ) ;
#14683 = LINE ( 'NONE', #22094, #15579 ) ;
#14684 = TOROIDAL_SURFACE ( 'NONE', #21600, 8.000000000000014211, 2.000000000000000000 ) ;
#14685 = ADVANCED_FACE ( 'NONE', ( #16349 ), #21681, .T. ) ;
#14686 = STYLED_ITEM ( 'NONE', ( #12007 ), #17421 ) ;
#14687 = CARTESIAN_POINT ( 'NONE',  ( 92.35396912051041340, 79.82103140542857034, -31.19620131593210388 ) ) ;
#14688 = LINE ( 'NONE', #5800, #9972 ) ;
#14689 = AXIS2_PLACEMENT_3D ( 'NONE', #13776, #1816, #14002 ) ;
#14690 = CARTESIAN_POINT ( 'NONE',  ( -90.40889375659911309, 78.43035437438882695, 33.17122784026039994 ) ) ;
#14691 = DIRECTION ( 'NONE',  ( -0.9999164797902017066, -6.965998958219365988E-18, 0.01292414190464157356 ) ) ;
#14692 = ORIENTED_EDGE ( 'NONE', *, *, #7534, .T. ) ;
#14693 = FACE_BOUND ( 'NONE', #129, .T. ) ;
#14694 = CARTESIAN_POINT ( 'NONE',  ( 3.394710440985788669, 158.4152080300494561, 256.6440692010450562 ) ) ;
#14695 = CARTESIAN_POINT ( 'NONE',  ( -14.88208367441968072, 180.3442769117117166, 312.4626966567733461 ) ) ;
#14696 = ORIENTED_EDGE ( 'NONE', *, *, #18879, .T. ) ;
#14697 = ORIENTED_EDGE ( 'NONE', *, *, #9581, .F. ) ;
#14698 = CARTESIAN_POINT ( 'NONE',  ( 106.2089377515399065, 72.00000000000000000, 28.62973177816241588 ) ) ;
#14699 = EDGE_CURVE ( 'NONE', #1745, #1664, #1303, .T. ) ;
#14700 = VECTOR ( 'NONE', #19719, 1000.000000000000000 ) ;
#14701 = VECTOR ( 'NONE', #14659, 1000.000000000000227 ) ;
#14702 = DIRECTION ( 'NONE',  ( -7.125109674364534776E-05, 0.9999848031710252272, -0.005512562950849704026 ) ) ;
#14703 = EDGE_CURVE ( 'NONE', #1627, #3659, #190, .T. ) ;
#14704 = ORIENTED_EDGE ( 'NONE', *, *, #21966, .T. ) ;
#14705 = CARTESIAN_POINT ( 'NONE',  ( -34.11225069749754368, 94.37751527644309135, 83.07029434066950557 ) ) ;
#14706 = AXIS2_PLACEMENT_3D ( 'NONE', #8458, #15506, #12159 ) ;
#14707 = CARTESIAN_POINT ( 'NONE',  ( -35.41995824635180412, 106.0982379271226677, 199.8585325857761177 ) ) ;
#14708 = EDGE_LOOP ( 'NONE', ( #7979, #2788 ) ) ;
#14709 = EDGE_CURVE ( 'NONE', #18446, #4308, #3088, .T. ) ;
#14710 = EDGE_LOOP ( 'NONE', ( #15868, #14933, #2389, #18769 ) ) ;
#14711 = DIRECTION ( 'NONE',  ( 0.8588562297929587253, 0.3902276408394437790, -0.3317956673477015506 ) ) ;
#14712 = EDGE_CURVE ( 'NONE', #7332, #4443, #19245, .T. ) ;
#14713 = CARTESIAN_POINT ( 'NONE',  ( 0.9903141991953918755, 165.4223666312992975, 76.61874151893944429 ) ) ;
#14714 = ORIENTED_EDGE ( 'NONE', *, *, #1131, .F. ) ;
#14715 = CARTESIAN_POINT ( 'NONE',  ( 0.000000000000000000, 1.999999999999998224, 0.000000000000000000 ) ) ;
#14716 = ORIENTED_EDGE ( 'NONE', *, *, #2520, .T. ) ;
#14717 = DIRECTION ( 'NONE',  ( -0.01292394549866737220, -0.005513023399721000799, -0.9999012842304692006 ) ) ;
#14718 = CARTESIAN_POINT ( 'NONE',  ( 51.42455095033975709, 113.4816418249608034, -44.85744920025983618 ) ) ;
#14719 = CARTESIAN_POINT ( 'NONE',  ( 162.0000000000000000, 0.000000000000000000, 2.222801351277976832E-12 ) ) ;
#14720 = AXIS2_PLACEMENT_3D ( 'NONE', #11675, #3052, #16978 ) ;
#14721 = AXIS2_PLACEMENT_3D ( 'NONE', #7840, #9204, #13035 ) ;
#14722 = CARTESIAN_POINT ( 'NONE',  ( -41.41899454747574083, 166.0889136240115249, 277.1829612759436827 ) ) ;
#14723 = AXIS2_PLACEMENT_3D ( 'NONE', #22082, #4528, #9470 ) ;
#14724 = CARTESIAN_POINT ( 'NONE',  ( 19.87979702288915718, 182.8092583941872533, 318.2062520007012267 ) ) ;
#14725 = CARTESIAN_POINT ( 'NONE',  ( -64.14629883989944403, 91.30780077822167584, 66.46930053661340310 ) ) ;
#14726 = EDGE_CURVE ( 'NONE', #12292, #8665, #2391, .T. ) ;
#14727 = VECTOR ( 'NONE', #15266, 1000.000000000000000 ) ;
#14728 = ORIENTED_EDGE ( 'NONE', *, *, #6401, .F. ) ;
#14729 = LINE ( 'NONE', #14612, #20188 ) ;
#14730 = CARTESIAN_POINT ( 'NONE',  ( -88.18706637290718220, 88.71869973106700513, 50.32066939225164504 ) ) ;
#14731 = ADVANCED_FACE ( 'NONE', ( #8357, #1030 ), #5019, .T. ) ;
#14732 = DIRECTION ( 'NONE',  ( 0.1884548733085491812, 0.000000000000000000, 0.9820818503191365290 ) ) ;
#14733 = VECTOR ( 'NONE', #21047, 1000.000000000000114 ) ;
#14735 = EDGE_LOOP ( 'NONE', ( #3709, #1723, #18398 ) ) ;
#14734 = ORIENTED_EDGE ( 'NONE', *, *, #2794, .T. ) ;
#14736 = TOROIDAL_SURFACE ( 'NONE', #785, 110.5000000000000000, 2.000000000000000000 ) ;
#14737 = CARTESIAN_POINT ( 'NONE',  ( -51.81996628516554182, 111.6265379432125684, -46.67980995128849031 ) ) ;
#14738 = ORIENTED_EDGE ( 'NONE', *, *, #13051, .F. ) ;
#14739 = DIRECTION ( 'NONE',  ( 0.01292394549866695240, 0.005513023399725255208, 0.9999012842304693116 ) ) ;
#14740 = CONICAL_SURFACE ( 'NONE', #9210, 3.047499999999998987, 1.047197551196594523 ) ;
#14741 = CARTESIAN_POINT ( 'NONE',  ( -75.30975508861040169, 94.90914755154933857, 80.17755788556743823 ) ) ;
#14742 = CARTESIAN_POINT ( 'NONE',  ( 91.62437796271727564, 95.44063823554748183, 60.86849236629024773 ) ) ;
#14743 = DIRECTION ( 'NONE',  ( 0.000000000000000000, 0.000000000000000000, 1.000000000000000000 ) ) ;
#14744 = CARTESIAN_POINT ( 'NONE',  ( 37.51330139321492396, 72.00000000000000000, -87.03232607370792095 ) ) ;
#14745 = CARTESIAN_POINT ( 'NONE',  ( -91.62437796271721879, 95.44063823554751025, -60.86849236629028326 ) ) ;
#14746 = ORIENTED_EDGE ( 'NONE', *, *, #18315, .T. ) ;
#14747 = ADVANCED_FACE ( 'NONE', ( #16892 ), #9871, .F. ) ;
#14748 = DIRECTION ( 'NONE',  ( -0.01292394549866738782, -0.005513023399720468239, -0.9999012842304692006 ) ) ;
#14749 = AXIS2_PLACEMENT_3D ( 'NONE', #18237, #16947, #20471 ) ;
#14750 = ORIENTED_EDGE ( 'NONE', *, *, #1370, .F. ) ;
#14751 = DIRECTION ( 'NONE',  ( -5.440186201345738641E-18, -1.000000000000000000, -1.334940939666364181E-17 ) ) ;
#14752 = CARTESIAN_POINT ( 'NONE',  ( -91.65137210734575035, 77.59584042966187667, -29.57018005965453611 ) ) ;
#14753 = CARTESIAN_POINT ( 'NONE',  ( -12.50473920891009882, 146.4814768226545141, 276.8334956993934384 ) ) ;
#14754 = CARTESIAN_POINT ( 'NONE',  ( -37.51330139321489554, 69.99999999999998579, 87.03232607370787832 ) ) ;
#14755 = LINE ( 'NONE', #16469, #1144 ) ;
#14756 = CARTESIAN_POINT ( 'NONE',  ( 43.10250357860363835, 95.91520285510637223, 84.25345810160554549 ) ) ;
#14757 = FACE_OUTER_BOUND ( 'NONE', #1742, .T. ) ;
#14758 = EDGE_LOOP ( 'NONE', ( #22103, #3142 ) ) ;
#14759 = CARTESIAN_POINT ( 'NONE',  ( -1.163172771417702700, 81.97459999999998104, -89.99248318111824574 ) ) ;
#14760 = EDGE_LOOP ( 'NONE', ( #10160, #8284, #16424, #2518 ) ) ;
#14761 = AXIS2_PLACEMENT_3D ( 'NONE', #20468, #15338, #11881 ) ;
#14762 = ORIENTED_EDGE ( 'NONE', *, *, #8333, .F. ) ;
#14763 = CARTESIAN_POINT ( 'NONE',  ( -80.05923150692979107, 75.13699351169597662, -4.065642694558678549 ) ) ;
#14764 = CARTESIAN_POINT ( 'NONE',  ( 13.85032138075246699, 137.5759562808229362, 104.3910387985238799 ) ) ;
#14765 = EDGE_CURVE ( 'NONE', #11360, #9297, #554, .T. ) ;
#14766 = AXIS2_PLACEMENT_3D ( 'NONE', #12925, #12462, #14771 ) ;
#14767 = DIRECTION ( 'NONE',  ( -0.005493774068846058074, 0.02859024303483492097, -0.9995761183870338629 ) ) ;
#14769 = VERTEX_POINT ( 'NONE', #4575 ) ;
#14768 = ORIENTED_EDGE ( 'NONE', *, *, #10213, .T. ) ;
#14770 = VERTEX_POINT ( 'NONE', #22349 ) ;
#14771 = DIRECTION ( 'NONE',  ( -7.125109674243555432E-05, 0.9999848031710253382, -0.005512562950850175003 ) ) ;
#14772 = DIRECTION ( 'NONE',  ( 7.125109674364534776E-05, -0.9999848031710252272, 0.005512562950849704893 ) ) ;
#14773 = VECTOR ( 'NONE', #18367, 1000.000000000000000 ) ;
#14774 = CARTESIAN_POINT ( 'NONE',  ( -39.99341017482546334, 93.41702043935060829, -83.07303732980588507 ) ) ;
#14775 = COLOUR_RGB ( '', 0.08235294, 0.09019608, 0.10196078) ;
#14776 = DIRECTION ( 'NONE',  ( -0.01292394549866731149, -0.005513023399720593139, -0.9999012842304692006 ) ) ;
#14777 = EDGE_CURVE ( 'NONE', #9718, #8189, #18168, .T. ) ;
#14778 = CARTESIAN_POINT ( 'NONE',  ( 52.34460878051607580, 84.99999999999997158, 26.32568957529409204 ) ) ;
#14779 = CARTESIAN_POINT ( 'NONE',  ( 17.24533165808599477, 186.5834384566230995, 277.7277893435518763 ) ) ;
#14780 = VECTOR ( 'NONE', #4922, 1000.000000000000000 ) ;
#14781 = CARTESIAN_POINT ( 'NONE',  ( 19.15828809225966722, 184.7089495515359943, 317.1432155856761028 ) ) ;
#14782 = DIRECTION ( 'NONE',  ( 0.1288482667915162305, 1.253717443260671224E-17, -0.9916643202943334900 ) ) ;
#14783 = CARTESIAN_POINT ( 'NONE',  ( 22.08632752877390359, 147.9377667753725802, 276.4622185031857384 ) ) ;
#14784 = VERTEX_POINT ( 'NONE', #11708 ) ;
#14785 = AXIS2_PLACEMENT_3D ( 'NONE', #11530, #22056, #17049 ) ;
#14786 = FACE_OUTER_BOUND ( 'NONE', #10838, .T. ) ;
#14787 = CARTESIAN_POINT ( 'NONE',  ( -5.135453193612369738, 87.00000000000001421, -93.02909119787791781 ) ) ;
#14788 = ORIENTED_EDGE ( 'NONE', *, *, #1938, .T. ) ;
#14790 = CARTESIAN_POINT ( 'NONE',  ( -22.66159625276162970, 324.6936785073799001, 307.5691494985305781 ) ) ;
#14789 = AXIS2_PLACEMENT_3D ( 'NONE', #15299, #8593, #18933 ) ;
#14791 = ORIENTED_EDGE ( 'NONE', *, *, #8058, .T. ) ;
#14792 = VECTOR ( 'NONE', #14242, 1000.000000000000000 ) ;
#14793 = AXIS2_PLACEMENT_3D ( 'NONE', #15103, #12718, #16300 ) ;
#14794 = CARTESIAN_POINT ( 'NONE',  ( 48.11994755510385602, 111.2501766408243498, -44.80243313535611804 ) ) ;
#14795 = CARTESIAN_POINT ( 'NONE',  ( -8.877829866301334860, 140.4778767860208291, 86.88480985406179968 ) ) ;
#14796 = EDGE_CURVE ( 'NONE', #19373, #6945, #7152, .T. ) ;
#14797 = ADVANCED_FACE ( 'NONE', ( #1155 ), #22244, .T. ) ;
#14798 =( NAMED_UNIT ( * ) PLANE_ANGLE_UNIT ( ) SI_UNIT ( $, .RADIAN. ) );
#14799 = CARTESIAN_POINT ( 'NONE',  ( -63.92582232734818604, 91.13550884953522768, 66.60804284595937474 ) ) ;
#14800 = LINE ( 'NONE', #11103, #3424 ) ;
#14801 = DIRECTION ( 'NONE',  ( -0.9999164797902015955, -6.965998958219364448E-18, 0.01292414190464157182 ) ) ;
#14802 = ORIENTED_EDGE ( 'NONE', *, *, #8342, .F. ) ;
#14803 = CARTESIAN_POINT ( 'NONE',  ( -69.43142427201328815, 92.58578643762699301, 85.31868097644080251 ) ) ;
#14804 = CARTESIAN_POINT ( 'NONE',  ( -159.9866367664323832, 0.000000000000000000, 2.067862704742662316 ) ) ;
#14805 = CARTESIAN_POINT ( 'NONE',  ( -19.28847592064633787, 309.3375565838056787, 328.6122914246403184 ) ) ;
#14806 = VECTOR ( 'NONE', #16328, 999.9999999999998863 ) ;
#14807 = CARTESIAN_POINT ( 'NONE',  ( -40.95677474166659238, 106.8061942917681790, 71.46866982798410106 ) ) ;
#14808 = VECTOR ( 'NONE', #7716, 1000.000000000000114 ) ;
#14809 = CARTESIAN_POINT ( 'NONE',  ( 91.77247882320288852, 77.19421037201389879, -31.29629296515013692 ) ) ;
#14810 = DIRECTION ( 'NONE',  ( 0.9999164797902015955, 0.000000000000000000, -0.01292414190464118845 ) ) ;
#14811 =( LENGTH_UNIT ( ) NAMED_UNIT ( * ) SI_UNIT ( .MILLI., .METRE. ) );
#14812 = ORIENTED_EDGE ( 'NONE', *, *, #21972, .T. ) ;
#14813 = LINE ( 'NONE', #11453, #5559 ) ;
#14814 = DIRECTION ( 'NONE',  ( -0.9999164797902015955, -2.001050586450178695E-22, 0.01292414190464131335 ) ) ;
#14815 = CARTESIAN_POINT ( 'NONE',  ( -10.63046908155944692, 187.2581710861182671, 308.2567892644384528 ) ) ;
#14816 = VERTEX_POINT ( 'NONE', #13674 ) ;
#14817 = ORIENTED_EDGE ( 'NONE', *, *, #2190, .F. ) ;
#14818 = ADVANCED_FACE ( 'NONE', ( #8024 ), #15515, .T. ) ;
#14819 = DIRECTION ( 'NONE',  ( -2.025474946048326158E-22, 1.000000000000000000, -1.876735158486679638E-22 ) ) ;
#14820 = AXIS2_PLACEMENT_3D ( 'NONE', #197, #15834, #7078 ) ;
#14821 = AXIS2_PLACEMENT_3D ( 'NONE', #19586, #13976, #19472 ) ;
#14822 = CYLINDRICAL_SURFACE ( 'NONE', #2671, 1.999999999999997780 ) ;
#14823 = CARTESIAN_POINT ( 'NONE',  ( -38.45083117249132698, 165.6589964890517592, 273.1465725822631612 ) ) ;
#14824 = DIRECTION ( 'NONE',  ( -0.01292394549866731843, -0.005513023399720594006, -0.9999012842304693116 ) ) ;
#14825 = AXIS2_PLACEMENT_3D ( 'NONE', #2765, #1163, #6540 ) ;
#14826 = AXIS2_PLACEMENT_3D ( 'NONE', #1559, #3499, #20948 ) ;
#14827 = ORIENTED_EDGE ( 'NONE', *, *, #18596, .T. ) ;
#14828 = CARTESIAN_POINT ( 'NONE',  ( 0.8743530591963382115, 70.00000000000002842, -98.80339646031046641 ) ) ;
#14829 = CARTESIAN_POINT ( 'NONE',  ( -11.36765543714179394, 183.1705039132345973, 306.0958062668278785 ) ) ;
#14830 = DIRECTION ( 'NONE',  ( 0.000000000000000000, 0.000000000000000000, 1.000000000000000000 ) ) ;
#14831 = ORIENTED_EDGE ( 'NONE', *, *, #10058, .T. ) ;
#14832 = CYLINDRICAL_SURFACE ( 'NONE', #15591, 4.500000000000006217 ) ;
#14833 = DIRECTION ( 'NONE',  ( 7.125109674364536131E-05, -0.9999848031710253382, 0.005512562950849705760 ) ) ;
#14834 = CARTESIAN_POINT ( 'NONE',  ( -24.45368655303012417, 89.79783256935353108, 79.21683296045429756 ) ) ;
#14835 = AXIS2_PLACEMENT_3D ( 'NONE', #1775, #14202, #19566 ) ;
#14836 = VERTEX_POINT ( 'NONE', #20654 ) ;
#14837 = AXIS2_PLACEMENT_3D ( 'NONE', #7076, #12486, #195 ) ;
#14838 = DIRECTION ( 'NONE',  ( 0.01292394549866740169, 0.005513023399719847208, 0.9999012842304693116 ) ) ;
#14839 = CARTESIAN_POINT ( 'NONE',  ( -0.1457028305847436478, 81.85301533877176894, -80.78463022974997898 ) ) ;
#14840 = ORIENTED_EDGE ( 'NONE', *, *, #13297, .T. ) ;
#14841 = AXIS2_PLACEMENT_3D ( 'NONE', #10256, #17058, #1321 ) ;
#14842 = CIRCLE ( 'NONE', #17779, 6.499999999999985789 ) ;
#14843 = EDGE_CURVE ( 'NONE', #11064, #17159, #5583, .T. ) ;
#14844 = DIRECTION ( 'NONE',  ( -0.6915547089979457995, 0.09853460026858232301, 0.7155718112200041281 ) ) ;
#14845 = CARTESIAN_POINT ( 'NONE',  ( -88.17134115317794851, 88.83281691486382670, 52.17357975332178910 ) ) ;
#14846 = EDGE_CURVE ( 'NONE', #17586, #8873, #15058, .T. ) ;
#14847 = SHAPE_DEFINITION_REPRESENTATION ( #3716, #15634 ) ;
#14848 = CIRCLE ( 'NONE', #3823, 95.00000000000004263 ) ;
#14850 = ORIENTED_EDGE ( 'NONE', *, *, #14078, .F. ) ;
#14849 = ORIENTED_EDGE ( 'NONE', *, *, #4314, .F. ) ;
#14851 = VECTOR ( 'NONE', #5277, 999.9999999999998863 ) ;
#14852 = DIRECTION ( 'NONE',  ( 0.9999164797902017066, 6.965998958219365988E-18, -0.01292414190464157356 ) ) ;
#14853 = CARTESIAN_POINT ( 'NONE',  ( -51.02393100784042446, 110.5294973102531770, -46.28750279846238413 ) ) ;
#14854 = ORIENTED_EDGE ( 'NONE', *, *, #8354, .F. ) ;
#14855 = CARTESIAN_POINT ( 'NONE',  ( -1.163172771417702700, 30.00000000000000711, -89.99248318111824574 ) ) ;
#14856 = DIRECTION ( 'NONE',  ( 2.025474946048326158E-22, -1.000000000000000000, 1.876735158486679638E-22 ) ) ;
#14857 = DIRECTION ( 'NONE',  ( -0.9999164797902015955, 0.000000000000000000, 0.01292414190464218071 ) ) ;
#14859 = CARTESIAN_POINT ( 'NONE',  ( -1.163172771417704698, 69.99999999999998579, -89.99248318111816047 ) ) ;
#14858 = APPLICATION_CONTEXT ( 'automotive_design' ) ;
#14860 = EDGE_CURVE ( 'NONE', #10313, #1614, #8154, .T. ) ;
#14861 = ORIENTED_EDGE ( 'NONE', *, *, #6425, .T. ) ;
#14862 = CARTESIAN_POINT ( 'NONE',  ( 34.23466015841589183, 93.68133903400143936, -83.10361438825003688 ) ) ;
#14863 = VERTEX_POINT ( 'NONE', #13449 ) ;
#14864 = DIRECTION ( 'NONE',  ( 7.125109674161246868E-05, -0.9999848031710252272, 0.005512562950850154186 ) ) ;
#14865 = DIRECTION ( 'NONE',  ( -1.000000000000000000, 0.000000000000000000, -1.387778780781444413E-14 ) ) ;
#14866 = VECTOR ( 'NONE', #15755, 1000.000000000000227 ) ;
#14867 = CARTESIAN_POINT ( 'NONE',  ( -3.863860647413861926, 143.2476736384784033, 275.3398486090524102 ) ) ;
#14868 = CARTESIAN_POINT ( 'NONE',  ( -10.81153106956454479, 70.35526451184087193, -89.75216824834804186 ) ) ;
#14869 = EDGE_CURVE ( 'NONE', #7249, #9044, #20418, .T. ) ;
#14870 = CARTESIAN_POINT ( 'NONE',  ( 39.99665919160806027, 170.0000000000000284, -0.5169656761856848970 ) ) ;
#14871 = LINE ( 'NONE', #13697, #2412 ) ;
#14872 = AXIS2_PLACEMENT_3D ( 'NONE', #5667, #12587, #2116 ) ;
#14873 = CARTESIAN_POINT ( 'NONE',  ( -51.47772934420782320, 111.2940323025706846, -46.56188176222278940 ) ) ;
#14874 = ORIENTED_EDGE ( 'NONE', *, *, #7971, .F. ) ;
#14875 = VECTOR ( 'NONE', #17759, 1000.000000000000114 ) ;
#14876 = FACE_OUTER_BOUND ( 'NONE', #11149, .T. ) ;
#14877 = ORIENTED_EDGE ( 'NONE', *, *, #15408, .F. ) ;
#14878 = EDGE_CURVE ( 'NONE', #3984, #18513, #8878, .T. ) ;
#14879 = CARTESIAN_POINT ( 'NONE',  ( -105.4334892372614121, 72.00000000000000000, 31.36525700924958926 ) ) ;
#14880 = CARTESIAN_POINT ( 'NONE',  ( -90.10851746777733240, 88.45132993515882447, 52.79029924855479550 ) ) ;
#14881 = ADVANCED_FACE ( 'NONE', ( #19382 ), #9031, .T. ) ;
#14882 = AXIS2_PLACEMENT_3D ( 'NONE', #8634, #19322, #10263 ) ;
#14883 = FACE_OUTER_BOUND ( 'NONE', #15463, .T. ) ;
#14884 = EDGE_CURVE ( 'NONE', #800, #11619, #306, .T. ) ;
#14885 = EDGE_LOOP ( 'NONE', ( #16590, #6875, #17230, #7752 ) ) ;
#14886 = CARTESIAN_POINT ( 'NONE',  ( -37.08415557685306396, 105.5218503240047454, 92.65813065591969178 ) ) ;
#14887 = CARTESIAN_POINT ( 'NONE',  ( -52.56676294784124792, 113.4816418249608034, -43.51333844217711544 ) ) ;
#14888 = CARTESIAN_POINT ( 'NONE',  ( -41.00865927789263310, 166.2639521169525665, 308.9298270502609967 ) ) ;
#14889 = CARTESIAN_POINT ( 'NONE',  ( 47.39940051867662874, 108.3707227317548529, -46.77744129239903259 ) ) ;
#14890 = CARTESIAN_POINT ( 'NONE',  ( 3.600049111542418689, 166.5356125545590373, 278.5290088303507332 ) ) ;
#14891 = DIRECTION ( 'NONE',  ( -0.9250486434174662875, -0.3795887553195633202, 0.01404934683357507604 ) ) ;
#14892 = ORIENTED_EDGE ( 'NONE', *, *, #18557, .T. ) ;
#14893 = ORIENTED_EDGE ( 'NONE', *, *, #853, .F. ) ;
#14894 =( NAMED_UNIT ( * ) SI_UNIT ( $, .STERADIAN. ) SOLID_ANGLE_UNIT ( ) );
#14895 = DIRECTION ( 'NONE',  ( 0.01292414190463832269, 0.000000000000000000, 0.9999164797902017066 ) ) ;
#14896 = CARTESIAN_POINT ( 'NONE',  ( 19.03050207494622725, 183.6302965638845137, 319.7390526622639300 ) ) ;
#14897 = EDGE_CURVE ( 'NONE', #379, #11828, #6320, .T. ) ;
#14898 = CARTESIAN_POINT ( 'NONE',  ( 73.81922676008082362, 96.21294322789840692, -81.74793453868313975 ) ) ;
#14899 = FACE_OUTER_BOUND ( 'NONE', #3029, .T. ) ;
#14900 = EDGE_CURVE ( 'NONE', #8178, #4043, #840, .T. ) ;
#14901 = ORIENTED_EDGE ( 'NONE', *, *, #7695, .F. ) ;
#14902 = PRODUCT ( 'Hex Nut', 'Hex Nut', '', ( #5730 ) ) ;
#14903 = DIRECTION ( 'NONE',  ( 0.009188991635466048358, -0.7031977391749438810, 0.7109349492407661675 ) ) ;
#14904 = CARTESIAN_POINT ( 'NONE',  ( 9.142505149400548703, 81.99999999999998579, -88.65345271381772818 ) ) ;
#14905 = ORIENTED_EDGE ( 'NONE', *, *, #5913, .T. ) ;
#14906 = DIRECTION ( 'NONE',  ( 0.000000000000000000, 0.000000000000000000, 1.000000000000000000 ) ) ;
#14907 = ORIENTED_EDGE ( 'NONE', *, *, #15113, .T. ) ;
#14908 = CARTESIAN_POINT ( 'NONE',  ( 48.79856628852573408, 112.2275063344195303, -44.81659300615380204 ) ) ;
#14909 = DIRECTION ( 'NONE',  ( -0.01292394549866731669, -0.005513023399720593139, -0.9999012842304692006 ) ) ;
#14910 = ADVANCED_FACE ( 'NONE', ( #3303 ), #3646, .F. ) ;
#14911 = ORIENTED_EDGE ( 'NONE', *, *, #10520, .T. ) ;
#14912 = CARTESIAN_POINT ( 'NONE',  ( -49.61360656010212722, 118.9155345184949653, 166.8635573802473857 ) ) ;
#14913 = CARTESIAN_POINT ( 'NONE',  ( 76.93439171139391419, 75.08638595516887904, 3.060657608357647774 ) ) ;
#14914 = SHAPE_REPRESENTATION ( 'Socket Head Cap Screw', ( #6292 ), #7016 ) ;
#14915 = DIRECTION ( 'NONE',  ( -0.8588562297929586142, -0.3902276408394423912, 0.3317956673477029383 ) ) ;
#14916 = CIRCLE ( 'NONE', #14544, 7.499999999999992006 ) ;
#14917 = CARTESIAN_POINT ( 'NONE',  ( 75.07406019263973462, 75.07594612489205588, 2.843253612283983767 ) ) ;
#14918 = CARTESIAN_POINT ( 'NONE',  ( -39.39497909003006981, 91.17157287525388654, 85.51628863845817818 ) ) ;
#14919 = ORIENTED_EDGE ( 'NONE', *, *, #5685, .F. ) ;
#14920 = CARTESIAN_POINT ( 'NONE',  ( 9.796239224404398982, 190.0809038477337651, 274.9155399994040181 ) ) ;
#14921 = DIRECTION ( 'NONE',  ( -0.9999999898465624648, -0.0001425000279005267183, 7.855523118142308109E-07 ) ) ;
#14922 = CARTESIAN_POINT ( 'NONE',  ( 17.46492942237984991, 175.6255473142593644, 113.2354285962226328 ) ) ;
#14923 = CARTESIAN_POINT ( 'NONE',  ( -39.75561905526965489, 107.1788419875363303, 71.78347329497708529 ) ) ;
#14924 = CARTESIAN_POINT ( 'NONE',  ( 90.65029634199440522, 79.17021053268413766, -29.01211804384235649 ) ) ;
#14925 = EDGE_CURVE ( 'NONE', #1532, #2916, #15625, .T. ) ;
#14926 = EDGE_CURVE ( 'NONE', #2396, #20375, #3431, .T. ) ;
#14928 = CARTESIAN_POINT ( 'NONE',  ( 7.015576680412771715, 166.1312609306101535, 81.53744875812694204 ) ) ;
#14927 = CARTESIAN_POINT ( 'NONE',  ( -1.163172771417702700, 69.99999999999998579, -89.99248318111824574 ) ) ;
#14929 = PLANE ( 'NONE',  #5171 ) ;
#14930 = ORIENTED_EDGE ( 'NONE', *, *, #21843, .T. ) ;
#14931 = DIRECTION ( 'NONE',  ( 0.01292394549866738782, 0.005513023399720468239, 0.9999012842304692006 ) ) ;
#14932 = CARTESIAN_POINT ( 'NONE',  ( -13.76919743346306646, 180.5356774100213784, 310.4380730639882131 ) ) ;
#14933 = ORIENTED_EDGE ( 'NONE', *, *, #20150, .T. ) ;
#14934 = AXIS2_PLACEMENT_3D ( 'NONE', #3195, #12063, #1497 ) ;
#14935 = ORIENTED_EDGE ( 'NONE', *, *, #2609, .T. ) ;
#14936 = CARTESIAN_POINT ( 'NONE',  ( 12.55221694283142853, 189.7895332285891641, 307.7358867228051622 ) ) ;
#14937 = DIRECTION ( 'NONE',  ( -0.8981428216242088869, 0.000000000000000000, -0.4397038457472307593 ) ) ;
#14938 = DIRECTION ( 'NONE',  ( 0.009760756503427813965, -0.9999378516499565217, 0.005387065077611106687 ) ) ;
#14939 = VERTEX_POINT ( 'NONE', #17693 ) ;
#14940 = ORIENTED_EDGE ( 'NONE', *, *, #12756, .T. ) ;
#14941 = CARTESIAN_POINT ( 'NONE',  ( 12.79778896233726471, 190.5038093453642603, 307.8472338899999841 ) ) ;
#14942 = CARTESIAN_POINT ( 'NONE',  ( -13.22370634329071848, 181.0695397079195459, 321.5726873589048864 ) ) ;
#14943 = ADVANCED_FACE ( 'NONE', ( #17343 ), #7412, .T. ) ;
#14944 = EDGE_LOOP ( 'NONE', ( #17118, #22162, #12229 ) ) ;
#14945 = CARTESIAN_POINT ( 'NONE',  ( -44.75576560912451640, 168.6025580852140706, 19.18675944895310082 ) ) ;
#14946 = DIRECTION ( 'NONE',  ( -0.9999164797902015955, -6.965998958219364448E-18, 0.01292414190464157182 ) ) ;
#14947 = CARTESIAN_POINT ( 'NONE',  ( 16.25138420224134705, 87.34880441414898655, 76.12342506946350795 ) ) ;
#14948 = VERTEX_POINT ( 'NONE', #12050 ) ;
#14949 = PLANE ( 'NONE',  #20366 ) ;
#14950 = CARTESIAN_POINT ( 'NONE',  ( -9.296350947641979445, 186.8092295296417262, 307.8158422510384185 ) ) ;
#14951 = EDGE_LOOP ( 'NONE', ( #115, #16594, #1334, #18316 ) ) ;
#14952 = DIRECTION ( 'NONE',  ( -7.125109674025824596E-05, 0.9999848031710253382, -0.005512562950849464634 ) ) ;
#14953 = CARTESIAN_POINT ( 'NONE',  ( -89.44439933878480531, 89.11516110322091322, 51.58556162172175164 ) ) ;
#14954 = CONTEXT_DEPENDENT_SHAPE_REPRESENTATION ( #7338, #5532 ) ;
#14955 = ORIENTED_EDGE ( 'NONE', *, *, #1948, .F. ) ;
#14956 = DIRECTION ( 'NONE',  ( 0.000000000000000000, 0.000000000000000000, 1.000000000000000000 ) ) ;
#14957 = CARTESIAN_POINT ( 'NONE',  ( -52.26439264322070954, 113.4816418191338414, -43.51724664528359909 ) ) ;
#14958 = EDGE_LOOP ( 'NONE', ( #12943, #9801, #11869, #6594 ) ) ;
#14959 = DIRECTION ( 'NONE',  ( 9.912705577010319386E-17, 0.000000000000000000, 1.000000000000000000 ) ) ;
#14960 = DIRECTION ( 'NONE',  ( 0.01292394549866738261, 0.005513023399722618428, 0.9999012842304692006 ) ) ;
#14961 = CARTESIAN_POINT ( 'NONE',  ( 67.44333765613016851, 145.1911235850904234, 33.86722133266570722 ) ) ;
#14962 = FACE_OUTER_BOUND ( 'NONE', #19645, .T. ) ;
#14963 = ORIENTED_EDGE ( 'NONE', *, *, #1776, .T. ) ;
#14964 = CARTESIAN_POINT ( 'NONE',  ( 35.60052562348057137, 93.98891615189143067, -83.40426226564440526 ) ) ;
#14965 = VERTEX_POINT ( 'NONE', #3770 ) ;
#14966 = CARTESIAN_POINT ( 'NONE',  ( -6.596016192384672294, 157.5478644388096541, 81.76070674735760235 ) ) ;
#14967 = CARTESIAN_POINT ( 'NONE',  ( -92.02038759195845330, 72.00000000000000000, 63.24214162404745565 ) ) ;
#14968 = CARTESIAN_POINT ( 'NONE',  ( -1.163172771417702700, 81.99999999999998579, -89.99248318111824574 ) ) ;
#14969 = DIRECTION ( 'NONE',  ( -0.01104128644981183967, -0.5197558313507629757, -0.8542435049623791077 ) ) ;
#14970 = EDGE_CURVE ( 'NONE', #8421, #7828, #1599, .T. ) ;
#14971 = AXIS2_PLACEMENT_3D ( 'NONE', #12554, #3476, #21255 ) ;
#14972 = DIRECTION ( 'NONE',  ( -0.009088227368120585167, -0.7109943316365089361, -0.7031390079522393810 ) ) ;
#14973 = DIRECTION ( 'NONE',  ( 0.009760756503427210282, -0.9999378516499566327, 0.005387065077606872227 ) ) ;
#14974 = ORIENTED_EDGE ( 'NONE', *, *, #14046, .F. ) ;
#14975 = DIRECTION ( 'NONE',  ( 7.125109674160325297E-05, -0.9999848031710253382, 0.005512562950849327591 ) ) ;
#14976 = EDGE_LOOP ( 'NONE', ( #12789, #3242, #3278 ) ) ;
#14977 = SURFACE_SIDE_STYLE ('',( #7947 ) ) ;
#14978 = EDGE_CURVE ( 'NONE', #9627, #4929, #4835, .T. ) ;
#14979 = CARTESIAN_POINT ( 'NONE',  ( -88.16225667628052065, 88.12760352708744449, 53.01283023165030528 ) ) ;
#14980 = EDGE_CURVE ( 'NONE', #1058, #4221, #20621, .T. ) ;
#14981 = DIRECTION ( 'NONE',  ( 0.01292394549866637994, 0.005513023399719273882, 0.9999012842304692006 ) ) ;
#14982 = ORIENTED_EDGE ( 'NONE', *, *, #22384, .F. ) ;
#14983 = AXIS2_PLACEMENT_3D ( 'NONE', #3661, #10569, #19173 ) ;
#14984 = EDGE_CURVE ( 'NONE', #16331, #16712, #12295, .T. ) ;
#14985 = LINE ( 'NONE', #4612, #1895 ) ;
#14986 = CARTESIAN_POINT ( 'NONE',  ( -67.76708237988898986, 98.06134765687328070, 76.92491524063726160 ) ) ;
#14987 = DIRECTION ( 'NONE',  ( -7.125109674364534776E-05, 0.9999848031710252272, -0.005512562950849704893 ) ) ;
#14988 = CARTESIAN_POINT ( 'NONE',  ( 67.23320572660466610, 192.1022009597330680, 17.60971032628828681 ) ) ;
#14989 = CARTESIAN_POINT ( 'NONE',  ( -36.86384537466776834, 93.14505924924313263, 85.22952222962540247 ) ) ;
#14990 = ORIENTED_EDGE ( 'NONE', *, *, #8209, .T. ) ;
#14991 = ORIENTED_EDGE ( 'NONE', *, *, #15159, .F. ) ;
#14992 = LINE ( 'NONE', #13492, #10636 ) ;
#14993 = DIRECTION ( 'NONE',  ( -0.9999164797902015955, -2.001050586450177755E-22, 0.01292414190464177999 ) ) ;
#14994 = CARTESIAN_POINT ( 'NONE',  ( 19.62580668441758647, 184.0217288607373121, 316.1492713539591364 ) ) ;
#14995 = CARTESIAN_POINT ( 'NONE',  ( 51.78636885665599010, 152.2590373701828241, 256.0525387646090394 ) ) ;
#14996 = VECTOR ( 'NONE', #11396, 999.9999999999998863 ) ;
#14997 = EDGE_CURVE ( 'NONE', #7423, #15641, #10551, .T. ) ;
#14998 = ADVANCED_FACE ( 'NONE', ( #21216 ), #12575, .T. ) ;
#14999 = LINE ( 'NONE', #21732, #13232 ) ;
#15000 = DIRECTION ( 'NONE',  ( 0.01292394549866738782, 0.005513023399720468239, 0.9999012842304692006 ) ) ;
#15001 = DIRECTION ( 'NONE',  ( -0.9999164797902017066, -6.965998958219365988E-18, 0.01292414190464157356 ) ) ;
#15002 = ORIENTED_EDGE ( 'NONE', *, *, #368, .F. ) ;
#15003 = CARTESIAN_POINT ( 'NONE',  ( -41.67747345744867715, 165.9786531560170033, 257.1849355913340673 ) ) ;
#15004 = ORIENTED_EDGE ( 'NONE', *, *, #13505, .T. ) ;
#15005 = EDGE_CURVE ( 'NONE', #12564, #11300, #1820, .T. ) ;
#15006 = DIRECTION ( 'NONE',  ( -7.125109674364534776E-05, 0.9999848031710252272, -0.005512562950849704893 ) ) ;
#15007 = EDGE_LOOP ( 'NONE', ( #1545, #18047, #2874, #15643 ) ) ;
#15008 = EDGE_CURVE ( 'NONE', #2643, #8739, #17318, .T. ) ;
#15009 = VECTOR ( 'NONE', #10246, 1000.000000000000000 ) ;
#15010 = VERTEX_POINT ( 'NONE', #18031 ) ;
#15011 = EDGE_CURVE ( 'NONE', #6632, #22379, #17650, .T. ) ;
#15012 = CARTESIAN_POINT ( 'NONE',  ( 77.82328986082669076, 75.11365078037778176, -5.652215941475883909 ) ) ;
#15013 = CARTESIAN_POINT ( 'NONE',  ( -91.01151104332689101, 70.28404947875058895, 61.80376916000803789 ) ) ;
#15014 = CIRCLE ( 'NONE', #5073, 2.000000000000004441 ) ;
#15015 = CARTESIAN_POINT ( 'NONE',  ( 82.26820226798385249, 75.18049222980359048, 4.790965612300991161 ) ) ;
#15016 =( REPRESENTATION_RELATIONSHIP ('NONE','NONE', #11808, #19567 ) REPRESENTATION_RELATIONSHIP_WITH_TRANSFORMATION ( #5475 )SHAPE_REPRESENTATION_RELATIONSHIP( ) );
#15017 = DIRECTION ( 'NONE',  ( 0.9232306267972765212, 0.000000000000000000, -0.3842462878721248920 ) ) ;
#15018 = ORIENTED_EDGE ( 'NONE', *, *, #4338, .T. ) ;
#15019 = CARTESIAN_POINT ( 'NONE',  ( 10.83543253063041689, 189.7684987719255503, 275.3551034107306350 ) ) ;
#15020 = ORIENTED_EDGE ( 'NONE', *, *, #15487, .T. ) ;
#15021 = DIRECTION ( 'NONE',  ( 0.8741796853632723963, 0.002667950166551805863, 0.4855952633007025732 ) ) ;
#15022 = CARTESIAN_POINT ( 'NONE',  ( 89.99012571735545407, 95.97180966979294681, -63.25964760396028908 ) ) ;
#15023 = DIRECTION ( 'NONE',  ( 1.396592535537253658E-14, -0.000000000000000000, 1.000000000000000000 ) ) ;
#15024 = EDGE_CURVE ( 'NONE', #17822, #18942, #4100, .T. ) ;
#15025 = CARTESIAN_POINT ( 'NONE',  ( 89.23446290093956179, 79.53212074382834373, -30.14913290299190862 ) ) ;
#15026 = CARTESIAN_POINT ( 'NONE',  ( -9.786139105534834570, 187.7140077023060485, 321.1629084044704996 ) ) ;
#15027 = FACE_OUTER_BOUND ( 'NONE', #2023, .T. ) ;
#15028 = ORIENTED_EDGE ( 'NONE', *, *, #1414, .F. ) ;
#15029 = AXIS2_PLACEMENT_3D ( 'NONE', #7460, #5833, #1956 ) ;
#15030 = DIRECTION ( 'NONE',  ( -0.9999164797902015955, -4.476705744456278510E-15, 0.01292414190463697134 ) ) ;
#15031 = ORIENTED_EDGE ( 'NONE', *, *, #21546, .F. ) ;
#15032 = CARTESIAN_POINT ( 'NONE',  ( -55.33808647217894361, 114.8068154851947753, 167.6347561330238420 ) ) ;
#15033 = CARTESIAN_POINT ( 'NONE',  ( -11.49837594199064839, 183.0688075479256440, 306.1363948905710117 ) ) ;
#15034 = VECTOR ( 'NONE', #2078, 1000.000000000000114 ) ;
#15035 = EDGE_LOOP ( 'NONE', ( #9824, #11507, #8984, #2555 ) ) ;
#15036 = ORIENTED_EDGE ( 'NONE', *, *, #16991, .T. ) ;
#15037 = SHAPE_REPRESENTATION ( 'Handle Handwheel Knob', ( #6292 ), #18057 ) ;
#15038 = CARTESIAN_POINT ( 'NONE',  ( -67.64952533873930918, 70.35418627987228035, 86.73849053056652281 ) ) ;
#15039 = EDGE_CURVE ( 'NONE', #15758, #8927, #14485, .T. ) ;
#15040 = LINE ( 'NONE', #14823, #21364 ) ;
#15041 = DIRECTION ( 'NONE',  ( 0.9999164797902015955, 2.044556590511377167E-15, -0.01292414190464178173 ) ) ;
#15042 = EDGE_LOOP ( 'NONE', ( #4313, #9289 ) ) ;
#15043 = FACE_OUTER_BOUND ( 'NONE', #1432, .T. ) ;
#15044 = ADVANCED_FACE ( 'NONE', ( #12980 ), #18246, .T. ) ;
#15045 = CARTESIAN_POINT ( 'NONE',  ( -15.51054658338874326, 177.8073622993804861, 315.7124409163076280 ) ) ;
#15046 = ORIENTED_EDGE ( 'NONE', *, *, #13747, .T. ) ;
#15047 = CARTESIAN_POINT ( 'NONE',  ( -106.2343493168401949, 77.75544475269062161, -28.53532068555761825 ) ) ;
#15048 = CARTESIAN_POINT ( 'NONE',  ( -41.14926644985963122, 168.6907664596094776, 35.14123791416483300 ) ) ;
#15049 = DIRECTION ( 'NONE',  ( 0.1296504907605101897, 0.005475273188901850878, 0.9915446392518421082 ) ) ;
#15050 = ORIENTED_EDGE ( 'NONE', *, *, #16541, .F. ) ;
#15051 = LINE ( 'NONE', #9761, #16008 ) ;
#15052 = TOROIDAL_SURFACE ( 'NONE', #17239, 4.000000000000000000, 2.000000000000000000 ) ;
#15053 = FACE_OUTER_BOUND ( 'NONE', #22141, .T. ) ;
#15054 = CIRCLE ( 'NONE', #10346, 2.999999999999994227 ) ;
#15055 = ORIENTED_EDGE ( 'NONE', *, *, #1876, .T. ) ;
#15056 = UNCERTAINTY_MEASURE_WITH_UNIT (LENGTH_MEASURE( 1.000000000000000082E-05 ), #2065, 'distance_accuracy_value', 'NONE');
#15057 = CARTESIAN_POINT ( 'NONE',  ( -10.85572812182527613, 106.4999831797793775, 127.2949928129576733 ) ) ;
#15058 = LINE ( 'NONE', #22017, #18423 ) ;
#15059 = EDGE_CURVE ( 'NONE', #9820, #22544, #12947, .T. ) ;
#15060 = CIRCLE ( 'NONE', #376, 2.000000000000005329 ) ;
#15061 = APPLICATION_PROTOCOL_DEFINITION ( 'draft international standard', 'automotive_design', 1998, #6173 ) ;
#15062 = ADVANCED_FACE ( 'NONE', ( #21544 ), #3879, .F. ) ;
#15063 = VERTEX_POINT ( 'NONE', #21449 ) ;
#15064 = DIRECTION ( 'NONE',  ( 1.000000000000000000, 0.000000000000000000, -2.449293598294699019E-16 ) ) ;
#15065 = CARTESIAN_POINT ( 'NONE',  ( 91.73057767193266443, 77.20311952920094711, -31.31041951043028604 ) ) ;
#15066 = ORIENTED_EDGE ( 'NONE', *, *, #22525, .F. ) ;
#15067 = CARTESIAN_POINT ( 'NONE',  ( 26.54786300933031740, 169.3445808681009623, 324.2912630757292050 ) ) ;
#15068 = CARTESIAN_POINT ( 'NONE',  ( 18.16752390460396072, 176.4987325792368154, 90.21926235406634476 ) ) ;
#15069 = AXIS2_PLACEMENT_3D ( 'NONE', #20020, #9458, #2354 ) ;
#15070 = CARTESIAN_POINT ( 'NONE',  ( 14.14224087380716455, 105.6999953372425409, 126.9762993157022777 ) ) ;
#15071 = PRODUCT ( 'Hex Screw', 'Hex Screw', '', ( #16683 ) ) ;
#15072 = DIRECTION ( 'NONE',  ( 0.000000000000000000, 0.000000000000000000, 1.000000000000000000 ) ) ;
#15073 =( GEOMETRIC_REPRESENTATION_CONTEXT ( 3 ) GLOBAL_UNCERTAINTY_ASSIGNED_CONTEXT ( ( #5540 ) ) GLOBAL_UNIT_ASSIGNED_CONTEXT ( ( #14086, #1675, #15693 ) ) REPRESENTATION_CONTEXT ( 'NONE', 'WORKASPACE' ) );
#15074 = DIRECTION ( 'NONE',  ( -0.01292414190464137060, 0.000000000000000000, -0.9999164797902015955 ) ) ;
#15075 = ORIENTED_EDGE ( 'NONE', *, *, #11581, .T. ) ;
#15076 = PLANE ( 'NONE',  #11741 ) ;
#15077 = EDGE_LOOP ( 'NONE', ( #13749, #316, #6906, #4874 ) ) ;
#15078 = DIRECTION ( 'NONE',  ( -0.9999164797902017066, -1.471961700026549794E-14, 0.01292414190464131508 ) ) ;
#15079 = DIRECTION ( 'NONE',  ( -0.000000000000000000, -1.000000000000000000, 0.000000000000000000 ) ) ;
#15080 = PRODUCT_DEFINITION_FORMATION_WITH_SPECIFIED_SOURCE ( 'ANY', '', #15851, .NOT_KNOWN. ) ;
#15081 = CARTESIAN_POINT ( 'NONE',  ( 93.23587179807657321, 34.61572286322119396, 30.79757858250317071 ) ) ;
#15082 = FACE_OUTER_BOUND ( 'NONE', #7774, .T. ) ;
#15083 = VERTEX_POINT ( 'NONE', #12738 ) ;
#15084 = FACE_OUTER_BOUND ( 'NONE', #1962, .T. ) ;
#15085 = PRESENTATION_STYLE_ASSIGNMENT (( #2992 ) ) ;
#15086 = ORIENTED_EDGE ( 'NONE', *, *, #20473, .T. ) ;
#15087 = DIRECTION ( 'NONE',  ( 2.081668171172166620E-14, 1.000000000000000000, 0.000000000000000000 ) ) ;
#15088 = DIRECTION ( 'NONE',  ( 0.01292394549866743812, 0.005513023399720639109, 0.9999012842304693116 ) ) ;
#15089 = VERTEX_POINT ( 'NONE', #5815 ) ;
#15090 = ORIENTED_EDGE ( 'NONE', *, *, #4704, .T. ) ;
#15091 = AXIS2_PLACEMENT_3D ( 'NONE', #8978, #21260, #15673 ) ;
#15092 = LINE ( 'NONE', #4373, #6563 ) ;
#15093 = VECTOR ( 'NONE', #15829, 1000.000000000000114 ) ;
#15094 = EDGE_CURVE ( 'NONE', #9339, #12252, #11345, .T. ) ;
#15095 = CARTESIAN_POINT ( 'NONE',  ( -88.16354289163604108, 88.27034599685696037, 52.90680319025804579 ) ) ;
#15096 = VECTOR ( 'NONE', #16506, 1000.000000000000000 ) ;
#15097 = CARTESIAN_POINT ( 'NONE',  ( 55.40268456415108744, 1.999999999999998224, 113.1659955246503557 ) ) ;
#15098 = EDGE_LOOP ( 'NONE', ( #5907, #5682, #10773 ) ) ;
#15099 = ORIENTED_EDGE ( 'NONE', *, *, #4460, .F. ) ;
#15100 = CIRCLE ( 'NONE', #11047, 6.000000000000000888 ) ;
#15101 = CARTESIAN_POINT ( 'NONE',  ( -1.362186893977295590E-13, 18.00000000000000355, 9.999999999999994671 ) ) ;
#15102 = DIRECTION ( 'NONE',  ( 0.9909299940865188283, -0.1338359446631172955, -0.01207007604876741101 ) ) ;
#15103 = CARTESIAN_POINT ( 'NONE',  ( -1.163172771417702700, 81.99999999999998579, -89.99248318111824574 ) ) ;
#15104 = DIRECTION ( 'NONE',  ( 2.025474946048326158E-22, -1.000000000000000000, 1.876735158486679638E-22 ) ) ;
#15105 = CARTESIAN_POINT ( 'NONE',  ( -71.06083360305757424, 91.87225009003576304, -83.96645210693647243 ) ) ;
#15106 = ORIENTED_EDGE ( 'NONE', *, *, #9193, .F. ) ;
#15107 = CARTESIAN_POINT ( 'NONE',  ( -49.61330349940486428, 114.6621811589122757, 166.8870046147178812 ) ) ;
#15108 = B_SPLINE_CURVE_WITH_KNOTS ( 'NONE', 3,
 ( #21479, #1981, #8971, #10830, #17854, #21250, #2434, #10933, #21580, #601, #18071, #2090, #2319, #9074, #9318, #7592 ),
 .UNSPECIFIED., .F., .F.,
 ( 4, 2, 2, 2, 2, 2, 2, 4 ),
 ( 0.000000000000000000, 0.0008607555596716533631, 0.001291133339507492730, 0.001721511119343332097, 0.002151888899179171463, 0.002582266679015010613, 0.003012644458850850197, 0.003443022238686689347 ),
 .UNSPECIFIED. ) ;
#15109 = FACE_OUTER_BOUND ( 'NONE', #17827, .T. ) ;
#15110 = CARTESIAN_POINT ( 'NONE',  ( 19.91008402892363094, 183.5677589090103652, 315.0360073274616752 ) ) ;
#15111 = CARTESIAN_POINT ( 'NONE',  ( 93.17671387018316409, 79.04398536104953621, 26.22064129356657602 ) ) ;
#15112 = CIRCLE ( 'NONE', #13271, 96.00000000000000000 ) ;
#15113 = EDGE_CURVE ( 'NONE', #1333, #558, #9635, .T. ) ;
#15114 = CARTESIAN_POINT ( 'NONE',  ( -7.227204710067946181, 144.2888362340090396, 276.0193614813773593 ) ) ;
#15115 = DIRECTION ( 'NONE',  ( 0.000000000000000000, 0.000000000000000000, 1.000000000000000000 ) ) ;
#15116 = AXIS2_PLACEMENT_3D ( 'NONE', #7935, #15078, #1049 ) ;
#15117 = B_SPLINE_CURVE_WITH_KNOTS ( 'NONE', 3,
 ( #3928, #12352, #10948, #2213, #7380, #10726, #9094, #7265, #3593, #385, #504, #8744, #14424, #8990, #273, #7507, #10603, #5314, #21057, #17628, #14302, #21271, #14535, #5196, #12234, #3490, #10506, #17517, #14076, #7046, #15800, #41, #1882, #166, #7163, #7850, #730, #14646, #21720, #19766 ),
 .UNSPECIFIED., .F., .F.,
 ( 4, 2, 2, 2, 2, 2, 2, 2, 2, 2, 2, 2, 2, 2, 2, 2, 2, 2, 2, 4 ),
 ( 0.004439741376687713660, 0.005757347133595717287, 0.007074952890503720046, 0.008392558647411722805, 0.009710164404319727299, 0.01102777016122773006, 0.01168657303968165945, 0.01234537591813558710, 0.01300417879658951822, 0.01366298167504344588, 0.01432178455349737700, 0.01498058743195130466, 0.01629819318885934037, 0.01761579894576737609, 0.02025101045958349263, 0.02156861621649154917, 0.02288622197339960918, 0.02420382773030766571, 0.02486263060876169745, 0.02552143348721572919 ),
 .UNSPECIFIED. ) ;
#15118 = AXIS2_PLACEMENT_3D ( 'NONE', #18633, #11637, #2893 ) ;
#15119 = CARTESIAN_POINT ( 'NONE',  ( -49.99582398951010731, 170.0000000000000284, 0.6462070952320568828 ) ) ;
#15120 = CONICAL_SURFACE ( 'NONE', #21672, 9.000000000000001776, 1.047197551196594301 ) ;
#15121 = DIRECTION ( 'NONE',  ( 0.01292394549866731843, 0.005513023399720594006, 0.9999012842304693116 ) ) ;
#15122 = EDGE_LOOP ( 'NONE', ( #17853, #675, #17330, #11397, #12815, #2729, #9742, #2266 ) ) ;
#15123 = CARTESIAN_POINT ( 'NONE',  ( -6.558142562982950174, 188.9283497255633506, 275.5585268130429881 ) ) ;
#15124 = ORIENTED_EDGE ( 'NONE', *, *, #20185, .T. ) ;
#15125 = ORIENTED_EDGE ( 'NONE', *, *, #8072, .F. ) ;
#15126 = DIRECTION ( 'NONE',  ( 2.025474946048326158E-22, -1.000000000000000000, 1.876735158486679638E-22 ) ) ;
#15127 = DIRECTION ( 'NONE',  ( -0.009760756503427833047, 0.9999378516499565217, -0.005387065077611117095 ) ) ;
#15128 = AXIS2_PLACEMENT_3D ( 'NONE', #1508, #6552, #10123 ) ;
#15129 = ADVANCED_FACE ( 'NONE', ( #4098 ), #16536, .T. ) ;
#15130 = ORIENTED_EDGE ( 'NONE', *, *, #2863, .F. ) ;
#15131 = AXIS2_PLACEMENT_3D ( 'NONE', #3827, #3484, #17868 ) ;
#15132 = EDGE_CURVE ( 'NONE', #11414, #19968, #16426, .T. ) ;
#15133 = AXIS2_PLACEMENT_3D ( 'NONE', #1089, #15115, #22070 ) ;
#15134 = CARTESIAN_POINT ( 'NONE',  ( -49.28939966538133888, 107.5356485694709789, 70.72646220445905385 ) ) ;
#15135 = DIRECTION ( 'NONE',  ( 0.9232306267972776315, 0.000000000000000000, -0.3842462878721224495 ) ) ;
#15136 = CARTESIAN_POINT ( 'NONE',  ( 105.7487010638476335, 78.91327849199113587, -30.28586431387813960 ) ) ;
#15137 = LINE ( 'NONE', #2925, #18123 ) ;
#15138 = CIRCLE ( 'NONE', #8502, 2.000000000000005773 ) ;
#15139 = CARTESIAN_POINT ( 'NONE',  ( -1.163172771417702700, 81.99999999999998579, -89.99248318111824574 ) ) ;
#15140 = CARTESIAN_POINT ( 'NONE',  ( -91.23603883849614249, 72.00000000000000000, -30.82342686631250217 ) ) ;
#15141 = DIRECTION ( 'NONE',  ( -0.01292394549866737914, -0.005513023399721009472, -0.9999012842304692006 ) ) ;
#15142 = DIRECTION ( 'NONE',  ( 0.9999164797902017066, 6.965998958219367529E-18, -0.01292414190464157182 ) ) ;
#15143 = CARTESIAN_POINT ( 'NONE',  ( -54.20609587773724769, 114.2463865991324781, 172.5324734650571656 ) ) ;
#15144 = ADVANCED_FACE ( 'NONE', ( #7784 ), #14822, .T. ) ;
#15145 = CARTESIAN_POINT ( 'NONE',  ( 90.81765045018462956, 77.62753381201262926, -31.97827203367606330 ) ) ;
#15146 = DIRECTION ( 'NONE',  ( -2.025474946048326158E-22, 1.000000000000000000, -1.876735158486679638E-22 ) ) ;
#15147 = AXIS2_PLACEMENT_3D ( 'NONE', #17077, #1443, #1336 ) ;
#15148 = AXIS2_PLACEMENT_3D ( 'NONE', #15978, #216, #7100 ) ;
#15149 = PRESENTATION_LAYER_ASSIGNMENT (  '', '', ( #5933 ) ) ;
#15150 = EDGE_CURVE ( 'NONE', #6252, #3529, #18348, .T. ) ;
#15151 = ORIENTED_EDGE ( 'NONE', *, *, #5094, .F. ) ;
#15152 = DIRECTION ( 'NONE',  ( -1.000000000000000000, 0.000000000000000000, 9.912705577010318154E-17 ) ) ;
#15153 = CARTESIAN_POINT ( 'NONE',  ( -14.74258221042073913, 179.1459434199334169, 310.2631537442956642 ) ) ;
#15154 = EDGE_LOOP ( 'NONE', ( #13325, #18268, #17821 ) ) ;
#15155 = ORIENTED_EDGE ( 'NONE', *, *, #584, .T. ) ;
#15156 = VECTOR ( 'NONE', #11953, 1000.000000000000000 ) ;
#15157 =( REPRESENTATION_RELATIONSHIP ('NONE','NONE', #11808, #14914 ) REPRESENTATION_RELATIONSHIP_WITH_TRANSFORMATION ( #19946 )SHAPE_REPRESENTATION_RELATIONSHIP( ) );
#15158 = CARTESIAN_POINT ( 'NONE',  ( -68.71681667565952978, 72.00000000000000000, 85.89527988174785378 ) ) ;
#15159 = EDGE_CURVE ( 'NONE', #1217, #8332, #11927, .T. ) ;
#15160 = AXIS2_PLACEMENT_3D ( 'NONE', #6539, #20767, #19160 ) ;
#15162 = EDGE_CURVE ( 'NONE', #444, #21389, #1463, .T. ) ;
#15161 = VERTEX_POINT ( 'NONE', #20507 ) ;
#15163 = AXIS2_PLACEMENT_3D ( 'NONE', #16980, #2607, #16522 ) ;
#15164 = CARTESIAN_POINT ( 'NONE',  ( -1.421655609510530827, 45.00000000000000000, -109.9908127769221835 ) ) ;
#15165 = CARTESIAN_POINT ( 'NONE',  ( 58.87469064627514825, 145.0902203831571740, 105.9856375662876218 ) ) ;
#15166 = DIRECTION ( 'NONE',  ( 0.01292414190464131682, 1.902755938799531179E-22, 0.9999164797902017066 ) ) ;
#15167 = ORIENTED_EDGE ( 'NONE', *, *, #240, .T. ) ;
#15168 = DIRECTION ( 'NONE',  ( -0.8981428216242089979, 0.000000000000000000, -0.4397038457472307593 ) ) ;
#15169 = AXIS2_PLACEMENT_3D ( 'NONE', #12406, #21337, #14490 ) ;
#15170 = DIRECTION ( 'NONE',  ( -0.01292394549866741384, -0.005513023399720269613, -0.9999012842304692006 ) ) ;
#15171 = CARTESIAN_POINT ( 'NONE',  ( -59.98956404827792710, 126.2575686056374735, 47.61989594652990831 ) ) ;
#15172 = DIRECTION ( 'NONE',  ( -2.025474946048326393E-22, 1.000000000000000000, -1.876735158486679873E-22 ) ) ;
#15173 = ORIENTED_EDGE ( 'NONE', *, *, #11447, .T. ) ;
#15174 = CYLINDRICAL_SURFACE ( 'NONE', #16921, 126.0000000000000000 ) ;
#15175 = EDGE_CURVE ( 'NONE', #8292, #1407, #21875, .T. ) ;
#15176 = LINE ( 'NONE', #22128, #21102 ) ;
#15177 = VECTOR ( 'NONE', #6414, 1000.000000000000114 ) ;
#15178 = AXIS2_PLACEMENT_3D ( 'NONE', #2946, #15276, #20510 ) ;
#15179 = DIRECTION ( 'NONE',  ( -0.000000000000000000, -1.000000000000000000, -0.000000000000000000 ) ) ;
#15180 = DIRECTION ( 'NONE',  ( -0.01292394549866738608, -0.005513023399720699824, -0.9999012842304692006 ) ) ;
#15181 = ORIENTED_EDGE ( 'NONE', *, *, #15537, .T. ) ;
#15182 = CARTESIAN_POINT ( 'NONE',  ( 13.10989172854308293, 160.6801362231667269, 299.5102556940336171 ) ) ;
#15183 = CARTESIAN_POINT ( 'NONE',  ( 48.84321673125851504, 168.6907664596096765, 33.97806514274709144 ) ) ;
#15184 = EDGE_CURVE ( 'NONE', #2836, #22275, #4396, .T. ) ;
#15185 = AXIS2_PLACEMENT_3D ( 'NONE', #13415, #15142, #15586 ) ;
#15187 = ORIENTED_EDGE ( 'NONE', *, *, #16379, .T. ) ;
#15186 = ORIENTED_EDGE ( 'NONE', *, *, #1358, .T. ) ;
#15188 = ORIENTED_EDGE ( 'NONE', *, *, #19618, .T. ) ;
#15189 = DIRECTION ( 'NONE',  ( 2.025474946048326158E-22, -1.000000000000000000, 1.876735158486679638E-22 ) ) ;
#15190 = DIRECTION ( 'NONE',  ( 2.025474946048326158E-22, -1.000000000000000000, 1.876735158486679638E-22 ) ) ;
#15191 = ORIENTED_EDGE ( 'NONE', *, *, #9701, .F. ) ;
#15192 = CIRCLE ( 'NONE', #1592, 4.500000000000006217 ) ;
#15193 = CARTESIAN_POINT ( 'NONE',  ( 146.5000000000000000, 0.000000000000000000, -2.025191382850354537E-12 ) ) ;
#15194 = AXIS2_PLACEMENT_3D ( 'NONE', #3406, #15831, #7190 ) ;
#15195 = FACE_OUTER_BOUND ( 'NONE', #16150, .T. ) ;
#15196 = DIRECTION ( 'NONE',  ( 0.01292394549866739996, 0.005513023399721564584, 0.9999012842304692006 ) ) ;
#15197 = EDGE_LOOP ( 'NONE', ( #12642, #441, #3009, #1159, #16452 ) ) ;
#15198 = CARTESIAN_POINT ( 'NONE',  ( -0.003538370294055813436, 81.99999999999998579, -98.91746206376724615 ) ) ;
#15199 = DIRECTION ( 'NONE',  ( 0.000000000000000000, 0.000000000000000000, 1.000000000000000000 ) ) ;
#15200 = VERTEX_POINT ( 'NONE', #18802 ) ;
#15201 = CARTESIAN_POINT ( 'NONE',  ( -65.91440269377939387, 105.0000000000000000, -70.32555938675406537 ) ) ;
#15202 = LINE ( 'NONE', #3103, #9301 ) ;
#15203 = DIRECTION ( 'NONE',  ( -2.025474946048326158E-22, 1.000000000000000000, -1.876735158486679638E-22 ) ) ;
#15204 = DIRECTION ( 'NONE',  ( -7.125109674381882011E-05, 0.9999848031710253382, -0.005512562950849702291 ) ) ;
#15205 = ADVANCED_FACE ( 'NONE', ( #16865, #20167 ), #22109, .F. ) ;
#15206 = FACE_BOUND ( 'NONE', #9008, .T. ) ;
#15207 = FACE_OUTER_BOUND ( 'NONE', #3946, .T. ) ;
#15208 = ADVANCED_FACE ( 'NONE', ( #6620 ), #13647, .T. ) ;
#15209 = CIRCLE ( 'NONE', #9322, 2.000000000000001776 ) ;
#15210 = VERTEX_POINT ( 'NONE', #11688 ) ;
#15211 = DIRECTION ( 'NONE',  ( 0.9999164797902015955, 6.965998958219364448E-18, -0.01292414190464157182 ) ) ;
#15212 = DIRECTION ( 'NONE',  ( -7.125109674118361251E-05, 0.9999848031710253382, -0.005512562950849477644 ) ) ;
#15213 = ORIENTED_EDGE ( 'NONE', *, *, #1901, .T. ) ;
#15214 = AXIS2_PLACEMENT_3D ( 'NONE', #18425, #2693, #15556 ) ;
#15215 = TOROIDAL_SURFACE ( 'NONE', #4906, 93.00000000000000000, 2.000000000000000000 ) ;
#15216 =( LENGTH_UNIT ( ) NAMED_UNIT ( * ) SI_UNIT ( .MILLI., .METRE. ) );
#15217 = CARTESIAN_POINT ( 'NONE',  ( -88.16559194503513197, 88.46308404799054870, 52.72753900144177663 ) ) ;
#15219 = VERTEX_POINT ( 'NONE', #4438 ) ;
#15218 = EDGE_LOOP ( 'NONE', ( #14422, #21909 ) ) ;
#15220 = ORIENTED_EDGE ( 'NONE', *, *, #656, .F. ) ;
#15221 = DIRECTION ( 'NONE',  ( 0.01035335185279143318, 0.005513005182356926943, 0.9999312050732649393 ) ) ;
#15222 = CARTESIAN_POINT ( 'NONE',  ( 91.62437796271727564, 72.00000000000000000, 60.86849236629024773 ) ) ;
#15223 = CYLINDRICAL_SURFACE ( 'NONE', #2143, 8.000000000000000000 ) ;
#15224 = ORIENTED_EDGE ( 'NONE', *, *, #6888, .F. ) ;
#15225 = AXIS2_PLACEMENT_3D ( 'NONE', #16221, #11015, #14717 ) ;
#15226 = CARTESIAN_POINT ( 'NONE',  ( 64.42346518761236496, 113.4816418249608034, -45.02546304502017449 ) ) ;
#15227 = DIRECTION ( 'NONE',  ( 0.000000000000000000, 1.000000000000000000, -0.000000000000000000 ) ) ;
#15228 = CARTESIAN_POINT ( 'NONE',  ( -52.67340511173117079, 189.4880640929450237, -92.24003979316276514 ) ) ;
#15229 = VERTEX_POINT ( 'NONE', #8243 ) ;
#15230 = ORIENTED_EDGE ( 'NONE', *, *, #6568, .F. ) ;
#15231 = LINE ( 'NONE', #22287, #16181 ) ;
#15232 = CARTESIAN_POINT ( 'NONE',  ( 8.863278656984560300, 190.2950607885061061, 274.5252716332005321 ) ) ;
#15233 = LINE ( 'NONE', #20363, #2107 ) ;
#15234 = VECTOR ( 'NONE', #4539, 1000.000000000000114 ) ;
#15235 = CARTESIAN_POINT ( 'NONE',  ( -10.85626963016051150, 114.0998676838791681, 127.2530973345311907 ) ) ;
#15236 = VECTOR ( 'NONE', #20717, 1000.000000000000000 ) ;
#15237 = EDGE_CURVE ( 'NONE', #17518, #21242, #2504, .T. ) ;
#15238 = LINE ( 'NONE', #16946, #6267 ) ;
#15239 = DIRECTION ( 'NONE',  ( 1.000000000000000000, 0.000000000000000000, 0.000000000000000000 ) ) ;
#15240 = DIRECTION ( 'NONE',  ( 0.01292394549866740169, 0.005513023399720822990, 0.9999012842304693116 ) ) ;
#15241 = CARTESIAN_POINT ( 'NONE',  ( -64.03068742478980369, 99.72761617120355027, 75.41393764079656137 ) ) ;
#15242 = ORIENTED_EDGE ( 'NONE', *, *, #4272, .T. ) ;
#15243 = VECTOR ( 'NONE', #11732, 1000.000000000000227 ) ;
#15244 = CARTESIAN_POINT ( 'NONE',  ( -9.798971742014797925, 187.6828575582066492, 276.1705134504438774 ) ) ;
#15245 = ORIENTED_EDGE ( 'NONE', *, *, #19390, .T. ) ;
#15246 = CARTESIAN_POINT ( 'NONE',  ( -80.05923150692979107, 75.13699351169597662, -4.065642694558678549 ) ) ;
#15247 = AXIS2_PLACEMENT_3D ( 'NONE', #1277, #10211, #8264 ) ;
#15248 = EDGE_LOOP ( 'NONE', ( #10964, #1033, #12079, #22298 ) ) ;
#15249 = CYLINDRICAL_SURFACE ( 'NONE', #20832, 2.000000000000001776 ) ;
#15250 = CARTESIAN_POINT ( 'NONE',  ( 1.364373935098378649E-14, 105.0000000000000000, -9.836450281572198869E-15 ) ) ;
#15251 = CARTESIAN_POINT ( 'NONE',  ( -107.2806549642561436, 77.80407930632172508, 24.41717176243129828 ) ) ;
#15252 = CARTESIAN_POINT ( 'NONE',  ( -89.22767861003021039, 80.31838830481383695, -30.18953644180660234 ) ) ;
#15253 = CARTESIAN_POINT ( 'NONE',  ( -92.50365291375118204, 70.32755610701403270, -59.52398455131075394 ) ) ;
#15254 = CARTESIAN_POINT ( 'NONE',  ( 14.08299609623372639, 188.4741397916250207, 275.9973987394899950 ) ) ;
#15255 = ORIENTED_EDGE ( 'NONE', *, *, #9406, .F. ) ;
#15256 = CARTESIAN_POINT ( 'NONE',  ( -46.77031037318527495, 119.7725967263615985, 250.1981111634296155 ) ) ;
#15257 = CARTESIAN_POINT ( 'NONE',  ( 7.319796769195229480, 81.85301533877174052, -86.26971152178252567 ) ) ;
#15258 = CIRCLE ( 'NONE', #13759, 2.000000000000000000 ) ;
#15259 = PLANE ( 'NONE',  #15185 ) ;
#15260 = DIRECTION ( 'NONE',  ( 0.9999164797902015955, 2.001050586450179636E-22, -0.01292414190464084844 ) ) ;
#15261 = FACE_OUTER_BOUND ( 'NONE', #1171, .T. ) ;
#15262 = CARTESIAN_POINT ( 'NONE',  ( 92.89382307712753573, 70.12557134413806637, 58.91325363510484436 ) ) ;
#15263 = ORIENTED_EDGE ( 'NONE', *, *, #21858, .T. ) ;
#15264 = EDGE_CURVE ( 'NONE', #18464, #18018, #8000, .T. ) ;
#15265 = ORIENTED_EDGE ( 'NONE', *, *, #6112, .F. ) ;
#15266 = DIRECTION ( 'NONE',  ( -0.9999164797902015955, -6.965998958219364448E-18, 0.01292414190464157182 ) ) ;
#15267 = CARTESIAN_POINT ( 'NONE',  ( -10.24828629132402824, 187.6512746430315985, 308.1882031990034534 ) ) ;
#15268 = ORIENTED_EDGE ( 'NONE', *, *, #8933, .F. ) ;
#15269 = CARTESIAN_POINT ( 'NONE',  ( -4.352520608367785648, 189.6274523698270684, 275.0976271054587414 ) ) ;
#15270 = ORIENTED_EDGE ( 'NONE', *, *, #3930, .T. ) ;
#15271 = AXIS2_PLACEMENT_3D ( 'NONE', #15882, #17365, #5272 ) ;
#15272 = PRODUCT_DEFINITION_SHAPE ( 'NONE', 'NONE',  #22701 ) ;
#15273 = CARTESIAN_POINT ( 'NONE',  ( -68.50871000753471662, 71.18193548034264495, 86.06142760398536495 ) ) ;
#15274 = ADVANCED_FACE ( 'NONE', ( #6513 ), #15378, .T. ) ;
#15275 = EDGE_CURVE ( 'NONE', #16549, #19747, #22061, .T. ) ;
#15276 = DIRECTION ( 'NONE',  ( -0.01292394549866741384, -0.005513023399720269613, -0.9999012842304692006 ) ) ;
#15277 = CARTESIAN_POINT ( 'NONE',  ( 19.98859775871076039, 148.6042059346136455, 276.7049348957753523 ) ) ;
#15278 = EDGE_CURVE ( 'NONE', #6286, #19552, #9073, .T. ) ;
#15279 = DIRECTION ( 'NONE',  ( 0.9934404589540163366, 0.1135548637187057258, -0.01346653032743021922 ) ) ;
#15280 = FACE_OUTER_BOUND ( 'NONE', #19805, .T. ) ;
#15281 = ORIENTED_EDGE ( 'NONE', *, *, #9343, .F. ) ;
#15282 = DIRECTION ( 'NONE',  ( -0.01292394549866744159, -0.005513023399721009472, -0.9999012842304692006 ) ) ;
#15283 = CARTESIAN_POINT ( 'NONE',  ( 7.483496276596866892, 69.99999999999998579, -92.63956227386769626 ) ) ;
#15284 = AXIS2_PLACEMENT_3D ( 'NONE', #18178, #364, #14743 ) ;
#15285 = CARTESIAN_POINT ( 'NONE',  ( 19.42556530730579567, 136.7551719540686008, -44.57217540897067920 ) ) ;
#15286 = ORIENTED_EDGE ( 'NONE', *, *, #11482, .F. ) ;
#15287 = EDGE_CURVE ( 'NONE', #10931, #21200, #14568, .T. ) ;
#15288 = CARTESIAN_POINT ( 'NONE',  ( 45.23618318876806654, 176.1024441089967070, 17.98224245540398769 ) ) ;
#15289 = EDGE_CURVE ( 'NONE', #11233, #9564, #5447, .T. ) ;
#15290 = LINE ( 'NONE', #13214, #22193 ) ;
#15291 = ADVANCED_FACE ( 'NONE', ( #22546, #21084 ), #20846, .T. ) ;
#15292 = APPLICATION_CONTEXT ( 'automotive_design' ) ;
#15293 = LINE ( 'NONE', #16779, #5842 ) ;
#15294 = CARTESIAN_POINT ( 'NONE',  ( -109.9908127769221693, 169.9999999999999716, 1.421655609510535045 ) ) ;
#15295 = DIRECTION ( 'NONE',  ( 0.01292414190464523903, 0.000000000000000000, 0.9999164797902017066 ) ) ;
#15296 = EDGE_CURVE ( 'NONE', #9610, #22618, #5220, .T. ) ;
#15297 = PRODUCT_CONTEXT ( 'NONE', #12043, 'mechanical' ) ;
#15298 = ORIENTED_EDGE ( 'NONE', *, *, #21487, .F. ) ;
#15299 = CARTESIAN_POINT ( 'NONE',  ( -64.99457118636313169, 170.0000000000000284, 0.8400692238016805868 ) ) ;
#15300 = ADVANCED_FACE ( 'NONE', ( #12138 ), #1792, .F. ) ;
#15301 = CARTESIAN_POINT ( 'NONE',  ( 3.575103298931712636, 166.5249713112435188, 276.5989983650335375 ) ) ;
#15302 = DIRECTION ( 'NONE',  ( 0.000000000000000000, 0.000000000000000000, 1.000000000000000000 ) ) ;
#15303 = PLANE ( 'NONE',  #20630 ) ;
#15304 = ORIENTED_EDGE ( 'NONE', *, *, #16967, .F. ) ;
#15305 = DIRECTION ( 'NONE',  ( -0.9999164797902015955, 8.863511990578706951E-16, 0.01292414190464158050 ) ) ;
#15306 = CARTESIAN_POINT ( 'NONE',  ( -16.55537123980816716, 137.6150987469609674, 111.8845242446517858 ) ) ;
#15307 = ORIENTED_EDGE ( 'NONE', *, *, #6118, .T. ) ;
#15308 = DIRECTION ( 'NONE',  ( 0.8981428216242027807, -0.000000000000000000, -0.4397038457472431938 ) ) ;
#15309 = ORIENTED_EDGE ( 'NONE', *, *, #8645, .F. ) ;
#15310 = FACE_OUTER_BOUND ( 'NONE', #10818, .T. ) ;
#15311 =( BOUNDED_SURFACE ( )  B_SPLINE_SURFACE ( 3, 3, ( 
 ( #14671, #21624, #12949, #18221 ),
 ( #7755, #6034, #20032, #13732 ),
 ( #13616, #4858, #16958, #20599 ),
 ( #15464, #18987, #11776, #8416 ) ),
 .UNSPECIFIED., .F., .F., .T. ) 
 B_SPLINE_SURFACE_WITH_KNOTS ( ( 4, 4 ),
 ( 4, 4 ),
 ( 0.000000000000000000, 1.000000000000000000 ),
 ( 0.000000000000000000, 1.000000000000000000 ),
 .UNSPECIFIED. ) 
 GEOMETRIC_REPRESENTATION_ITEM ( )  RATIONAL_B_SPLINE_SURFACE ( (
 ( 1.000000000000000000, 0.5185431720251972854, 0.5185431720251972854, 1.000000000000000000),
 ( 0.8047378541243649375, 0.4172913195263986963, 0.4172913195263986963, 0.8047378541243649375),
 ( 0.8047378541243649375, 0.4172913195263986963, 0.4172913195263986963, 0.8047378541243649375),
 ( 1.000000000000000000, 0.5185431720251972854, 0.5185431720251972854, 1.000000000000000000) ) ) 
 REPRESENTATION_ITEM ( '' )  SURFACE ( )  );
#15312 = CARTESIAN_POINT ( 'NONE',  ( -90.82246629754762068, 169.9999999999999716, 1.173900486973953772 ) ) ;
#15313 = DIRECTION ( 'NONE',  ( 7.125109674364534776E-05, -0.9999848031710252272, 0.005512562950849704893 ) ) ;
#15314 = LINE ( 'NONE', #8171, #18347 ) ;
#15315 = EDGE_CURVE ( 'NONE', #10332, #17177, #8772, .T. ) ;
#15316 = DIRECTION ( 'NONE',  ( 0.01292394549866737741, 0.005513023399721125699, 0.9999012842304693116 ) ) ;
#15317 = CARTESIAN_POINT ( 'NONE',  ( -51.09536285208268680, 114.2865790591373099, 170.4582858439766255 ) ) ;
#15318 = VERTEX_POINT ( 'NONE', #22652 ) ;
#15319 = CARTESIAN_POINT ( 'NONE',  ( -63.92222308695259869, 94.02752048664899576, 83.80561885825630952 ) ) ;
#15320 = CYLINDRICAL_SURFACE ( 'NONE', #4101, 95.00000000000001421 ) ;
#15321 = ORIENTED_EDGE ( 'NONE', *, *, #7734, .F. ) ;
#15322 = CARTESIAN_POINT ( 'NONE',  ( -1.523404093792848135, 158.5871283748866745, 324.7134023609685869 ) ) ;
#15323 = CARTESIAN_POINT ( 'NONE',  ( -90.15472117445577283, 87.25778962232662650, 51.24158970824034043 ) ) ;
#15325 = ORIENTED_EDGE ( 'NONE', *, *, #3510, .F. ) ;
#15324 = ORIENTED_EDGE ( 'NONE', *, *, #14483, .T. ) ;
#15326 = EDGE_CURVE ( 'NONE', #5010, #6442, #12865, .T. ) ;
#15327 = PLANE ( 'NONE',  #21307 ) ;
#15328 = DIRECTION ( 'NONE',  ( -0.01292414190464217898, -1.902755938799531885E-22, -0.9999164797902015955 ) ) ;
#15329 = DIRECTION ( 'NONE',  ( -0.01292414190464218071, 9.204123485805280727E-39, -0.9999164797902015955 ) ) ;
#15330 = CARTESIAN_POINT ( 'NONE',  ( 82.21743679224594814, 104.4142135623730923, -73.65452789938869671 ) ) ;
#15331 = CARTESIAN_POINT ( 'NONE',  ( -88.42085790543279700, 80.22997387171260186, 32.23265953185128296 ) ) ;
#15332 = VECTOR ( 'NONE', #260, 1000.000000000000000 ) ;
#15333 = CARTESIAN_POINT ( 'NONE',  ( -51.82774057240565213, 118.9447701193097942, 172.1955447453271404 ) ) ;
#15334 = ORIENTED_EDGE ( 'NONE', *, *, #2216, .T. ) ;
#15335 = CYLINDRICAL_SURFACE ( 'NONE', #9906, 2.000000000000001332 ) ;
#15336 = CARTESIAN_POINT ( 'NONE',  ( -90.02055463237803679, 72.00000000000000000, 63.21629334023816682 ) ) ;
#15337 = CARTESIAN_POINT ( 'NONE',  ( 88.41758806590424058, 80.31838830481383695, -32.48564084813595798 ) ) ;
#15338 = DIRECTION ( 'NONE',  ( 7.125109674161246868E-05, -0.9999848031710252272, 0.005512562950850154186 ) ) ;
#15339 = CARTESIAN_POINT ( 'NONE',  ( -2.729922624342409065, 142.9577372919816582, 275.2229497859695471 ) ) ;
#15340 = B_SPLINE_CURVE_WITH_KNOTS ( 'NONE', 3,
 ( #8308, #22295, #17280, #1544 ),
 .UNSPECIFIED., .F., .F.,
 ( 4, 4 ),
 ( 0.000000000000000000, 0.001461243987308202949 ),
 .UNSPECIFIED. ) ;
#15341 = SHAPE_REPRESENTATION_RELATIONSHIP ( 'NONE' , 'NONE' ,  #15770, #15403 ) ;
#15342 = FILL_AREA_STYLE ('',( #4202 ) ) ;
#15343 = CARTESIAN_POINT ( 'NONE',  ( 26.69469236638542853, 189.4444907833431273, -101.1701348970736518 ) ) ;
#15344 = VERTEX_POINT ( 'NONE', #6947 ) ;
#15345 = CARTESIAN_POINT ( 'NONE',  ( -13.95214564498276211, 185.6760471167460480, 276.6996455583582701 ) ) ;
#15346 = ORIENTED_EDGE ( 'NONE', *, *, #11528, .T. ) ;
#15347 = EDGE_LOOP ( 'NONE', ( #4606, #18768 ) ) ;
#15348 = AXIS2_PLACEMENT_3D ( 'NONE', #8704, #1833, #9047 ) ;
#15349 = CARTESIAN_POINT ( 'NONE',  ( -88.73586072705668926, 70.68102025985758985, 62.80242633408442288 ) ) ;
#15351 = VERTEX_POINT ( 'NONE', #4995 ) ;
#15350 = EDGE_LOOP ( 'NONE', ( #19353, #20953, #18733, #8219 ) ) ;
#15352 = EDGE_CURVE ( 'NONE', #11013, #14948, #7070, .T. ) ;
#15353 = CARTESIAN_POINT ( 'NONE',  ( -162.0000000000000000, 1.999999999999998224, 3.967855629237425111E-14 ) ) ;
#15354 = CYLINDRICAL_SURFACE ( 'NONE', #1199, 5.100000000000000533 ) ;
#15355 = EDGE_CURVE ( 'NONE', #15063, #5284, #8662, .T. ) ;
#15356 = AXIS2_PLACEMENT_3D ( 'NONE', #17970, #16477, #16257 ) ;
#15357 = B_SPLINE_CURVE_WITH_KNOTS ( 'NONE', 3,
 ( #59, #7178, #5213, #17885, #3502, #2117, #17773, #17989, #403, #285, #3609, #13959, #8760, #2015, #14092, #17531, #7400, #9112 ),
 .UNSPECIFIED., .F., .F.,
 ( 4, 2, 2, 2, 2, 2, 2, 2, 4 ),
 ( 0.000000000000000000, 0.0008023074076923169054, 0.001604614815384633811, 0.002406922223076950716, 0.003209229630769267622, 0.004011537038461584527, 0.004813844446153901432, 0.005616151853846218338, 0.006418459261538535243 ),
 .UNSPECIFIED. ) ;
#15358 = CARTESIAN_POINT ( 'NONE',  ( 85.63487699384957352, 75.04022993534840680, 1.663697398266591909 ) ) ;
#15359 = DIRECTION ( 'NONE',  ( 0.01292394549866738782, 0.005513023399720468239, 0.9999012842304692006 ) ) ;
#15360 = DIRECTION ( 'NONE',  ( -0.01292394549866738608, -0.005513023399720699824, -0.9999012842304692006 ) ) ;
#15361 = FACE_OUTER_BOUND ( 'NONE', #14233, .T. ) ;
#15362 = CARTESIAN_POINT ( 'NONE',  ( 13.02962957137955335, 190.4272972286120478, 320.8494027134000817 ) ) ;
#15363 = CARTESIAN_POINT ( 'NONE',  ( 41.99976970163857715, 124.0006990541328804, -0.2892360642558610695 ) ) ;
#15364 = DIRECTION ( 'NONE',  ( 0.01292394549866742078, 0.005513023399720777019, 0.9999012842304693116 ) ) ;
#15365 = AXIS2_PLACEMENT_3D ( 'NONE', #7801, #9401, #4332 ) ;
#15366 = CARTESIAN_POINT ( 'NONE',  ( 90.40889375659914151, 78.43035437438882695, -33.17122784026044258 ) ) ;
#15367 = ORIENTED_EDGE ( 'NONE', *, *, #10604, .F. ) ;
#15368 = CARTESIAN_POINT ( 'NONE',  ( -40.43344728539147326, 106.8827357009993051, 71.53004524236550310 ) ) ;
#15369 = ORIENTED_EDGE ( 'NONE', *, *, #10604, .T. ) ;
#15370 = EDGE_LOOP ( 'NONE', ( #18990, #16476, #35, #21551 ) ) ;
#15371 = CARTESIAN_POINT ( 'NONE',  ( -39.02517588049546049, 94.68893737706953573, 84.08474196546899293 ) ) ;
#15372 = CARTESIAN_POINT ( 'NONE',  ( 0.000000000000000000, 45.00000000000000711, 0.000000000000000000 ) ) ;
#15373 = VERTEX_POINT ( 'NONE', #10526 ) ;
#15374 = CARTESIAN_POINT ( 'NONE',  ( 6.523188911928190059, 70.01899995639452356, -85.22790637956202886 ) ) ;
#15375 = CIRCLE ( 'NONE', #5066, 120.0000000000000000 ) ;
#15376 = ORIENTED_EDGE ( 'NONE', *, *, #9653, .T. ) ;
#15377 = VECTOR ( 'NONE', #12237, 999.9999999999998863 ) ;
#15378 = CYLINDRICAL_SURFACE ( 'NONE', #16981, 110.5324305509042233 ) ;
#15379 = EDGE_CURVE ( 'NONE', #2284, #18513, #12482, .T. ) ;
#15380 = DIRECTION ( 'NONE',  ( -0.01292394549866738608, -0.005513023399720699824, -0.9999012842304692006 ) ) ;
#15381 = CARTESIAN_POINT ( 'NONE',  ( -9.820930688317483614, 187.6915098723768267, 321.1605422340256837 ) ) ;
#15382 = CARTESIAN_POINT ( 'NONE',  ( 10.34070483759711401, 143.0898343825529935, 274.9390076312643032 ) ) ;
#15383 = ORIENTED_EDGE ( 'NONE', *, *, #15059, .T. ) ;
#15384 = LINE ( 'NONE', #1697, #8745 ) ;
#15385 = ORIENTED_EDGE ( 'NONE', *, *, #15664, .T. ) ;
#15386 = CARTESIAN_POINT ( 'NONE',  ( -38.68617183816869698, 163.9153776386440882, 273.1592279730091377 ) ) ;
#15387 = ORIENTED_EDGE ( 'NONE', *, *, #15989, .T. ) ;
#15388 = CARTESIAN_POINT ( 'NONE',  ( 107.2806549642561293, 77.80407930632178193, -24.41717176243149723 ) ) ;
#15389 = CIRCLE ( 'NONE', #17204, 1.999999999999997780 ) ;
#15390 = CARTESIAN_POINT ( 'NONE',  ( 12.16442896649338223, 187.7168230983759543, 322.9757373289252200 ) ) ;
#15391 = VERTEX_POINT ( 'NONE', #5339 ) ;
#15392 = DIRECTION ( 'NONE',  ( 0.7220859686467110405, -0.6917813203664554544, -0.005518937903674935030 ) ) ;
#15393 = EDGE_CURVE ( 'NONE', #18381, #6677, #7348, .T. ) ;
#15394 = ORIENTED_EDGE ( 'NONE', *, *, #16605, .F. ) ;
#15395 = LINE ( 'NONE', #10204, #11005 ) ;
#15396 = CARTESIAN_POINT ( 'NONE',  ( 39.18815798788130422, 105.5072037373731888, 91.67997329703011644 ) ) ;
#15397 = DIRECTION ( 'NONE',  ( 0.9999164797902015955, 0.000000000000000000, -0.01292414190464144692 ) ) ;
#15398 = CARTESIAN_POINT ( 'NONE',  ( -34.79726985247908999, 121.2962013336460814, 248.0347590154626971 ) ) ;
#15399 = CARTESIAN_POINT ( 'NONE',  ( -7.243839870924989377, 70.07661102881318982, -96.85699015411138646 ) ) ;
#15400 = VECTOR ( 'NONE', #3522, 999.9999999999998863 ) ;
#15401 = DIRECTION ( 'NONE',  ( -2.025474946048326158E-22, 1.000000000000000000, -1.876735158486679638E-22 ) ) ;
#15402 = DIRECTION ( 'NONE',  ( -0.01035335185279143318, -0.005513005182356926943, -0.9999312050732649393 ) ) ;
#15403 = ADVANCED_BREP_SHAPE_REPRESENTATION ( '', ( #17010, #6292 ), #7391 ) ;
#15404 = PRODUCT_CONTEXT ( 'NONE', #17182, 'mechanical' ) ;
#15405 = AXIS2_PLACEMENT_3D ( 'NONE', #2178, #14507, #10821 ) ;
#15406 = EDGE_CURVE ( 'NONE', #22002, #8420, #7188, .T. ) ;
#15407 = ORIENTED_EDGE ( 'NONE', *, *, #4998, .T. ) ;
#15408 = EDGE_CURVE ( 'NONE', #14017, #2340, #14217, .T. ) ;
#15409 = FACE_OUTER_BOUND ( 'NONE', #9950, .T. ) ;
#15410 = CYLINDRICAL_SURFACE ( 'NONE', #21898, 3.399999999999985700 ) ;
#15411 = LINE ( 'NONE', #3311, #20962 ) ;
#15412 = FACE_OUTER_BOUND ( 'NONE', #14304, .T. ) ;
#15413 = ORIENTED_EDGE ( 'NONE', *, *, #14584, .F. ) ;
#15414 = CARTESIAN_POINT ( 'NONE',  ( 79.99331838321626265, 55.99999999999999289, -1.033931352371318058 ) ) ;
#15415 = CARTESIAN_POINT ( 'NONE',  ( -10.85624112972181621, 113.6998737626107641, 127.2553023597115498 ) ) ;
#15416 = VERTEX_POINT ( 'NONE', #19469 ) ;
#15417 = CARTESIAN_POINT ( 'NONE',  ( 49.57492634055867597, 108.8066997800019351, -44.80776678329138463 ) ) ;
#15418 = ORIENTED_EDGE ( 'NONE', *, *, #170, .F. ) ;
#15419 = CARTESIAN_POINT ( 'NONE',  ( 92.46788464407293873, 79.04398536104962147, -28.62013883513330015 ) ) ;
#15420 = CARTESIAN_POINT ( 'NONE',  ( 106.1347175484142724, 70.98259407754899541, 28.90376667366504293 ) ) ;
#15421 = CARTESIAN_POINT ( 'NONE',  ( -9.064738643541179641, 105.7168211570308500, 130.3284763332909222 ) ) ;
#15422 = CIRCLE ( 'NONE', #13215, 8.000000000000012434 ) ;
#15423 = EDGE_CURVE ( 'NONE', #4756, #18327, #17047, .T. ) ;
#15424 = CYLINDRICAL_SURFACE ( 'NONE', #21385, 4.500000000000006217 ) ;
#15425 = FACE_OUTER_BOUND ( 'NONE', #13402, .T. ) ;
#15426 = VECTOR ( 'NONE', #12845, 1000.000000000000114 ) ;
#15427 = ORIENTED_EDGE ( 'NONE', *, *, #18497, .T. ) ;
#15428 = FACE_OUTER_BOUND ( 'NONE', #8922, .T. ) ;
#15429 = EDGE_CURVE ( 'NONE', #18692, #13491, #17893, .T. ) ;
#15430 = CYLINDRICAL_SURFACE ( 'NONE', #1889, 87.00000000000001421 ) ;
#15431 = VERTEX_POINT ( 'NONE', #642 ) ;
#15432 = PRESENTATION_STYLE_ASSIGNMENT (( #8388 ) ) ;
#15433 = CARTESIAN_POINT ( 'NONE',  ( -90.04453709701007824, 88.62965799390647703, 52.60395590584802505 ) ) ;
#15434 = ORIENTED_EDGE ( 'NONE', *, *, #10615, .F. ) ;
#15435 = EDGE_CURVE ( 'NONE', #14816, #12349, #16399, .T. ) ;
#15436 = CARTESIAN_POINT ( 'NONE',  ( -74.05286932419430457, 95.97475531906495405, 81.34035317851895286 ) ) ;
#15437 = CARTESIAN_POINT ( 'NONE',  ( 64.99457118636310327, 170.0000000000000284, -0.8400692238017243296 ) ) ;
#15438 = CARTESIAN_POINT ( 'NONE',  ( -53.12394241931270500, 114.6366640169135849, 162.3035455873394426 ) ) ;
#15439 = CARTESIAN_POINT ( 'NONE',  ( 41.61793149762840471, 72.00000000000000000, 86.46934588545650513 ) ) ;
#15440 = DIRECTION ( 'NONE',  ( -0.000000000000000000, -1.000000000000000000, -0.000000000000000000 ) ) ;
#15441 = CARTESIAN_POINT ( 'NONE',  ( -88.16157026904451754, 88.04290212818517602, 53.06700061362226961 ) ) ;
#15442 = EDGE_CURVE ( 'NONE', #18403, #20909, #14033, .T. ) ;
#15443 = CARTESIAN_POINT ( 'NONE',  ( -91.15750879531698558, 79.10636023297634267, 28.80946033575589027 ) ) ;
#15444 = CARTESIAN_POINT ( 'NONE',  ( -71.51920288841773754, 92.50622980579329635, -83.57642618781949295 ) ) ;
#15445 = ORIENTED_EDGE ( 'NONE', *, *, #952, .F. ) ;
#15446 = AXIS2_PLACEMENT_3D ( 'NONE', #3874, #3638, #21441 ) ;
#15447 = VERTEX_POINT ( 'NONE', #2242 ) ;
#15448 = PLANE ( 'NONE',  #18007 ) ;
#15449 = CARTESIAN_POINT ( 'NONE',  ( 1.421655609510571683, 69.99999999999998579, 109.9908127769221409 ) ) ;
#15450 = CARTESIAN_POINT ( 'NONE',  ( 91.41602376139165642, 79.08283919787463390, -28.73514828341266281 ) ) ;
#15451 = CARTESIAN_POINT ( 'NONE',  ( -2.322807172541347498, 69.99999999999998579, -81.06750429846923112 ) ) ;
#15452 = CYLINDRICAL_SURFACE ( 'NONE', #7346, 85.00000000000001421 ) ;
#15453 = ORIENTED_EDGE ( 'NONE', *, *, #18882, .T. ) ;
#15454 =( NAMED_UNIT ( * ) SI_UNIT ( $, .STERADIAN. ) SOLID_ANGLE_UNIT ( ) );
#15455 = CARTESIAN_POINT ( 'NONE',  ( -146.5000000000000000, 20.00000000000000000, -9.999999999999980460 ) ) ;
#15456 = B_SPLINE_CURVE_WITH_KNOTS ( 'NONE', 3,
 ( #1234, #13413, #8226, #1343, #15257, #22208, #6721, #13743 ),
 .UNSPECIFIED., .F., .F.,
 ( 4, 2, 2, 4 ),
 ( 0.005257893453559938333, 0.006567392922673252059, 0.007876892391786564918, 0.01049589133001322533 ),
 .UNSPECIFIED. ) ;
#15457 = CIRCLE ( 'NONE', #21628, 2.000000000000004441 ) ;
#15458 = VECTOR ( 'NONE', #16139, 1000.000000000000000 ) ;
#15459 = EDGE_CURVE ( 'NONE', #20375, #4427, #8101, .T. ) ;
#15460 = CARTESIAN_POINT ( 'NONE',  ( -64.01907823019016064, 100.1566401219223081, 76.31211912804367614 ) ) ;
#15461 = ORIENTED_EDGE ( 'NONE', *, *, #15275, .F. ) ;
#15462 = EDGE_LOOP ( 'NONE', ( #694, #17726, #9217 ) ) ;
#15463 = EDGE_LOOP ( 'NONE', ( #12327, #1, #19432, #6031 ) ) ;
#15464 = CARTESIAN_POINT ( 'NONE',  ( -19.03062446302745414, 99.74539563421258492, 75.12800353666801811 ) ) ;
#15466 = ORIENTED_EDGE ( 'NONE', *, *, #380, .F. ) ;
#15465 = ORIENTED_EDGE ( 'NONE', *, *, #220, .F. ) ;
#15467 = EDGE_CURVE ( 'NONE', #558, #15229, #9013, .T. ) ;
#15468 = CARTESIAN_POINT ( 'NONE',  ( 78.59956642649036951, 75.12824275668153007, -5.951310493065621543 ) ) ;
#15469 = CARTESIAN_POINT ( 'NONE',  ( -85.84563054365271739, 105.0000000000000142, -68.77965573371086805 ) ) ;
#15470 = CARTESIAN_POINT ( 'NONE',  ( 105.4334892372614405, 77.28905753105605925, -31.36525700924962834 ) ) ;
#15471 = AXIS2_PLACEMENT_3D ( 'NONE', #21510, #16732, #2466 ) ;
#15472 = CARTESIAN_POINT ( 'NONE',  ( 4.195452682864886818, 166.7895964344300239, 324.5942600080955458 ) ) ;
#15473 = AXIS2_PLACEMENT_3D ( 'NONE', #6999, #15754, #22259 ) ;
#15474 = CARTESIAN_POINT ( 'NONE',  ( 12.83169261137808981, 190.5749574533797954, 307.8498635260945662 ) ) ;
#15475 = ORIENTED_EDGE ( 'NONE', *, *, #20695, .F. ) ;
#15476 = CARTESIAN_POINT ( 'NONE',  ( 0.000000000000000000, 0.000000000000000000, -101.0000000000000000 ) ) ;
#15477 = LINE ( 'NONE', #13845, #12986 ) ;
#15478 = VECTOR ( 'NONE', #1070, 1000.000000000000114 ) ;
#15479 = DIRECTION ( 'NONE',  ( -0.01292394549866741384, -0.005513023399720269613, -0.9999012842304692006 ) ) ;
#15480 = CARTESIAN_POINT ( 'NONE',  ( -51.01306968729422664, 189.5926701885510397, -73.28584260091861324 ) ) ;
#15481 = VERTEX_POINT ( 'NONE', #16061 ) ;
#15482 = CARTESIAN_POINT ( 'NONE',  ( -10.85567112094788200, 105.6999953372425409, 127.2994028633183063 ) ) ;
#15483 = CIRCLE ( 'NONE', #12896, 2.000000000000004885 ) ;
#15484 = EDGE_CURVE ( 'NONE', #13772, #12349, #20932, .T. ) ;
#15485 = FACE_OUTER_BOUND ( 'NONE', #5286, .T. ) ;
#15486 = FACE_OUTER_BOUND ( 'NONE', #17482, .T. ) ;
#15487 = EDGE_CURVE ( 'NONE', #12735, #22296, #12714, .T. ) ;
#15488 = EDGE_LOOP ( 'NONE', ( #11890, #8977 ) ) ;
#15489 = CARTESIAN_POINT ( 'NONE',  ( -72.50839346369934901, 87.61416393227378308, 70.38952438936911449 ) ) ;
#15490 = ORIENTED_EDGE ( 'NONE', *, *, #11319, .F. ) ;
#15491 = AXIS2_PLACEMENT_3D ( 'NONE', #14421, #19327, #21380 ) ;
#15492 = AXIS2_PLACEMENT_3D ( 'NONE', #14048, #10580, #14398 ) ;
#15493 = CARTESIAN_POINT ( 'NONE',  ( -34.56761431633026405, 165.3940184766423158, 308.8513715559440698 ) ) ;
#15494 = PRODUCT_DEFINITION_CONTEXT ( 'detailed design', #752, 'design' ) ;
#15495 = CARTESIAN_POINT ( 'NONE',  ( -4.928638145297007611, 326.7208992129484955, 307.3934828099208403 ) ) ;
#15496 = DIRECTION ( 'NONE',  ( 0.009760756503427813965, -0.9999378516499565217, 0.005387065077607405654 ) ) ;
#15497 = DIRECTION ( 'NONE',  ( -0.9999164797902015955, -4.476705744456278510E-15, 0.01292414190464144692 ) ) ;
#15498 = ORIENTED_EDGE ( 'NONE', *, *, #9930, .F. ) ;
#15499 = CARTESIAN_POINT ( 'NONE',  ( -45.15312007873932032, 180.5703843163154261, 257.1494065962392597 ) ) ;
#15500 = AXIS2_PLACEMENT_3D ( 'NONE', #5153, #21129, #10460 ) ;
#15501 = AXIS2_PLACEMENT_3D ( 'NONE', #14378, #10807, #19622 ) ;
#15502 = CARTESIAN_POINT ( 'NONE',  ( 109.9590233273770679, 75.10625493178588385, 3.218332492612444362 ) ) ;
#15503 = DIRECTION ( 'NONE',  ( 0.01292394549866741384, 0.005513023399720270480, 0.9999012842304693116 ) ) ;
#15504 = ORIENTED_EDGE ( 'NONE', *, *, #13315, .F. ) ;
#15505 = EDGE_CURVE ( 'NONE', #4929, #12, #5129, .T. ) ;
#15506 = DIRECTION ( 'NONE',  ( -0.01292394549866741904, -0.005513023399720750131, -0.9999012842304692006 ) ) ;
#15507 = VECTOR ( 'NONE', #16358, 1000.000000000000000 ) ;
#15508 = CARTESIAN_POINT ( 'NONE',  ( 22.08632752877390359, 147.9377667753725802, 276.4622185031857384 ) ) ;
#15509 = DIRECTION ( 'NONE',  ( 0.01292394549866695240, 0.005513023399725255208, 0.9999012842304693116 ) ) ;
#15510 = CARTESIAN_POINT ( 'NONE',  ( 18.76359067764538935, 183.6785240391465948, 308.7090574097932176 ) ) ;
#15511 = DIRECTION ( 'NONE',  ( -7.125109674081160920E-05, 0.9999848031710253382, -0.005512562950849312846 ) ) ;
#15512 = CARTESIAN_POINT ( 'NONE',  ( -41.23999883161326352, 108.3652131041115467, 59.07127508922548031 ) ) ;
#15513 = TOROIDAL_SURFACE ( 'NONE', #14425, 20.50000000000000355, 2.000000000000000000 ) ;
#15514 = DIRECTION ( 'NONE',  ( 0.8981428216242088869, -0.000000000000000000, 0.4397038457472307593 ) ) ;
#15515 = CONICAL_SURFACE ( 'NONE', #1923, 3.309500000000006992, 0.7853981633974710386 ) ;
#15516 = CARTESIAN_POINT ( 'NONE',  ( 4.195452682864886818, 166.7895964344300239, 324.5942600080955458 ) ) ;
#15517 = ITEM_DEFINED_TRANSFORMATION ( 'NONE', 'NONE', #10662,  #6292 ) ;
#15518 = EDGE_LOOP ( 'NONE', ( #17957, #913, #12096, #16196 ) ) ;
#15519 = CARTESIAN_POINT ( 'NONE',  ( -48.56673365018540522, 108.3817487785542539, -43.53692110109250279 ) ) ;
#15520 = CARTESIAN_POINT ( 'NONE',  ( 21.11681448353495938, 180.4772689128619163, 86.27658307888856370 ) ) ;
#15521 = DIRECTION ( 'NONE',  ( -0.9999164797902015955, -6.965998958219364448E-18, 0.01292414190464157182 ) ) ;
#15522 = DIRECTION ( 'NONE',  ( -2.025474946048326393E-22, 1.000000000000000000, -1.876735158486679873E-22 ) ) ;
#15523 = ORIENTED_EDGE ( 'NONE', *, *, #9670, .F. ) ;
#15524 = CARTESIAN_POINT ( 'NONE',  ( -56.08207636726148593, 126.6021325681200551, 110.0736613710297007 ) ) ;
#15525 = CARTESIAN_POINT ( 'NONE',  ( -48.56675504324970660, 108.6819931279166838, -43.53857624212188426 ) ) ;
#15526 = EDGE_LOOP ( 'NONE', ( #12147, #3003, #13041, #3174 ) ) ;
#15527 = CARTESIAN_POINT ( 'NONE',  ( -90.17340840076944630, 87.01269140061864960, 51.39028561451661403 ) ) ;
#15528 = VERTEX_POINT ( 'NONE', #18001 ) ;
#15529 = DIRECTION ( 'NONE',  ( -0.01292394549866745720, -0.005513023399720816918, -0.9999012842304692006 ) ) ;
#15530 = CARTESIAN_POINT ( 'NONE',  ( 106.1801133998813356, 71.34284122058939204, 28.73649967668635696 ) ) ;
#15531 = LINE ( 'NONE', #15421, #12173 ) ;
#15532 = AXIS2_PLACEMENT_3D ( 'NONE', #11468, #18353, #13323 ) ;
#15533 = EDGE_CURVE ( 'NONE', #21686, #5966, #4069, .T. ) ;
#15534 = AXIS2_PLACEMENT_3D ( 'NONE', #19879, #4145, #18189 ) ;
#15535 = FACE_BOUND ( 'NONE', #1306, .T. ) ;
#15536 = DIRECTION ( 'NONE',  ( 7.125109674364534776E-05, -0.9999848031710252272, 0.005512562950849704893 ) ) ;
#15537 = EDGE_CURVE ( 'NONE', #6614, #17745, #20024, .T. ) ;
#15538 = ORIENTED_EDGE ( 'NONE', *, *, #16350, .T. ) ;
#15539 = CARTESIAN_POINT ( 'NONE',  ( -13.57324918674249936, 183.7437101232661973, 276.7257079361987167 ) ) ;
#15540 = FACE_OUTER_BOUND ( 'NONE', #22219, .T. ) ;
#15541 = ORIENTED_EDGE ( 'NONE', *, *, #12940, .T. ) ;
#15542 = CARTESIAN_POINT ( 'NONE',  ( 90.02753699123907438, 71.81067029327459750, -63.20635338325894281 ) ) ;
#15543 = CARTESIAN_POINT ( 'NONE',  ( -89.94245242475622604, 88.81374284693771415, 52.36835579984497002 ) ) ;
#15544 = DIRECTION ( 'NONE',  ( -0.01292414190463830014, 0.000000000000000000, -0.9999164797902017066 ) ) ;
#15545 = AXIS2_PLACEMENT_3D ( 'NONE', #10164, #15359, #18994 ) ;
#15546 = ORIENTED_EDGE ( 'NONE', *, *, #7534, .F. ) ;
#15547 = AXIS2_PLACEMENT_3D ( 'NONE', #1133, #13649, #13533 ) ;
#15548 = EDGE_CURVE ( 'NONE', #10577, #6314, #11035, .T. ) ;
#15549 = ORIENTED_EDGE ( 'NONE', *, *, #1271, .F. ) ;
#15550 = DIRECTION ( 'NONE',  ( 7.125109674160258889E-05, -0.9999848031710252272, 0.005512562950849896580 ) ) ;
#15551 = DIRECTION ( 'NONE',  ( 0.01292394549866740169, 0.005513023399720822990, 0.9999012842304693116 ) ) ;
#15552 = CARTESIAN_POINT ( 'NONE',  ( 59.65012737619518646, 145.4210017871403977, 165.9797146201158000 ) ) ;
#15553 = FACE_OUTER_BOUND ( 'NONE', #14229, .T. ) ;
#15554 = CARTESIAN_POINT ( 'NONE',  ( 82.74584346241131527, 75.09876982897527853, 3.262718563837641472 ) ) ;
#15555 = CARTESIAN_POINT ( 'NONE',  ( 3.560643301544068162, 141.4162645520002002, 256.7356493073644401 ) ) ;
#15556 = DIRECTION ( 'NONE',  ( 0.01035335185279143318, 0.005513005182356926943, 0.9999312050732649393 ) ) ;
#15557 = ORIENTED_EDGE ( 'NONE', *, *, #16847, .T. ) ;
#15558 = EDGE_CURVE ( 'NONE', #6907, #18220, #8868, .T. ) ;
#15559 = ORIENTED_EDGE ( 'NONE', *, *, #18322, .T. ) ;
#15560 = SPHERICAL_SURFACE ( 'NONE', #15501, 2.000000000000000000 ) ;
#15561 = LINE ( 'NONE', #15906, #1262 ) ;
#15562 = CARTESIAN_POINT ( 'NONE',  ( 16.78462010304006924, 185.4095063563936492, 322.0781884391542462 ) ) ;
#15563 = CARTESIAN_POINT ( 'NONE',  ( 39.44739150791469484, 169.7656965055118974, -43.01277025598062664 ) ) ;
#15564 = CARTESIAN_POINT ( 'NONE',  ( -14.56978029430814203, 147.5825162344054888, 276.9379655111616785 ) ) ;
#15565 = ORIENTED_EDGE ( 'NONE', *, *, #21009, .T. ) ;
#15566 = CARTESIAN_POINT ( 'NONE',  ( -38.46706438352712354, 91.17157287525387233, 85.27439087629284131 ) ) ;
#15567 = CIRCLE ( 'NONE', #14835, 10.00000000000001421 ) ;
#15568 = EDGE_CURVE ( 'NONE', #1627, #18838, #16030, .T. ) ;
#15569 = VECTOR ( 'NONE', #968, 999.9999999999998863 ) ;
#15570 = EDGE_CURVE ( 'NONE', #3568, #1373, #7352, .T. ) ;
#15571 = CARTESIAN_POINT ( 'NONE',  ( -12.22010268980495518, 185.1830022132863292, 320.4502402655688797 ) ) ;
#15572 = ORIENTED_EDGE ( 'NONE', *, *, #13061, .T. ) ;
#15573 = ORIENTED_EDGE ( 'NONE', *, *, #8673, .F. ) ;
#15574 = EDGE_CURVE ( 'NONE', #10247, #1581, #4349, .T. ) ;
#15575 = CARTESIAN_POINT ( 'NONE',  ( -88.73541651539278519, 70.70236138404430903, 62.83679415258478684 ) ) ;
#15576 = AXIS2_PLACEMENT_3D ( 'NONE', #14967, #13466, #20437 ) ;
#15577 = VERTEX_POINT ( 'NONE', #2099 ) ;
#15578 = CARTESIAN_POINT ( 'NONE',  ( 51.64670511766545502, 84.99999999999997158, -27.66980033337678790 ) ) ;
#15579 = VECTOR ( 'NONE', #16750, 1000.000000000000114 ) ;
#15580 = TOROIDAL_SURFACE ( 'NONE', #19212, 97.00000000000004263, 2.000000000000000000 ) ;
#15581 = CARTESIAN_POINT ( 'NONE',  ( 63.61168800256650258, 69.99999999999997158, -107.8311325613533285 ) ) ;
#15582 = CARTESIAN_POINT ( 'NONE',  ( 0.000000000000000000, 25.00000000000000000, 0.000000000000000000 ) ) ;
#15583 = EDGE_CURVE ( 'NONE', #16395, #2309, #7156, .T. ) ;
#15584 = DIRECTION ( 'NONE',  ( 7.125109674403838460E-05, -0.9999848031710254492, 0.005512562950847868688 ) ) ;
#15585 = CARTESIAN_POINT ( 'NONE',  ( 48.54188012090998683, 169.3797848675314128, -113.1351015711598933 ) ) ;
#15586 = DIRECTION ( 'NONE',  ( -0.01292394549866739996, -0.005513023399721131770, -0.9999012842304692006 ) ) ;
#15587 = CARTESIAN_POINT ( 'NONE',  ( 11.56915902040221944, 187.8794726123035730, 307.7516944564536630 ) ) ;
#15588 = DIRECTION ( 'NONE',  ( -2.025474946048326158E-22, 1.000000000000000000, -1.876735158486679638E-22 ) ) ;
#15589 = EDGE_LOOP ( 'NONE', ( #10239, #6964, #13760, #19185 ) ) ;
#15590 = CARTESIAN_POINT ( 'NONE',  ( -58.38587380884935385, 114.5053385488661490, 162.9923002866045465 ) ) ;
#15591 = AXIS2_PLACEMENT_3D ( 'NONE', #18160, #9046, #2515 ) ;
#15592 = ADVANCED_FACE ( 'NONE', ( #6808 ), #11401, .F. ) ;
#15593 = LINE ( 'NONE', #13964, #18015 ) ;
#15594 = CARTESIAN_POINT ( 'NONE',  ( -8.586189643308495434, 185.3704654934846019, 305.1611493308044487 ) ) ;
#15595 = ORIENTED_EDGE ( 'NONE', *, *, #8715, .F. ) ;
#15596 = CARTESIAN_POINT ( 'NONE',  ( 5.986268468634207807, 69.99999999999998579, -84.52572088931836447 ) ) ;
#15597 = VERTEX_POINT ( 'NONE', #21264 ) ;
#15598 = B_SPLINE_CURVE_WITH_KNOTS ( 'NONE', 3,
 ( #14234, #21210, #17683, #19372, #18140, #3637, #12502, #318, #10774, #17805, #19486, #2041, #5700, #9026, #21098, #14351, #16078, #1931, #553, #2144, #7311, #14119, #9382, #12622, #19599, #2390, #662, #10991, #7552, #10650, #9143, #5353, #435, #3871, #16197, #14580 ),
 .UNSPECIFIED., .F., .F.,
 ( 4, 2, 2, 2, 2, 2, 2, 2, 2, 2, 2, 2, 2, 2, 2, 2, 2, 4 ),
 ( -5.999999999438343828E-08, 0.001317362229350502222, 0.002634784458700998883, 0.005269628917401928889, 0.006587051146752356812, 0.007904473376102786469, 0.009221895605453214392, 0.01053931783480364405, 0.01185674006415407197, 0.01251545117882927639, 0.01317416229350447908, 0.01383287340817968350, 0.01449158452285488619, 0.01580900675220515278, 0.01712642898155541590, 0.01844385121090567556, 0.01976127344025593868, 0.02107869566960620181 ),
 .UNSPECIFIED. ) ;
#15599 = VECTOR ( 'NONE', #9719, 1000.000000000000000 ) ;
#15600 = DIRECTION ( 'NONE',  ( -0.9999464000778708339, -1.417269118681738834E-05, 0.01035358732233848493 ) ) ;
#15601 = CIRCLE ( 'NONE', #9734, 4.200000000000005507 ) ;
#15602 = CARTESIAN_POINT ( 'NONE',  ( -2.015769147932460648, 327.0595725865082386, 308.7711644834471372 ) ) ;
#15603 = CARTESIAN_POINT ( 'NONE',  ( 15.95581455245526392, 145.6036739495936274, 276.5329765736894387 ) ) ;
#15604 = EDGE_CURVE ( 'NONE', #19271, #13521, #9183, .T. ) ;
#15605 = ORIENTED_EDGE ( 'NONE', *, *, #6496, .F. ) ;
#15606 = ADVANCED_FACE ( 'NONE', ( #20815 ), #12345, .T. ) ;
#15607 = CARTESIAN_POINT ( 'NONE',  ( -92.43457499998879712, 77.12912189496637438, 31.19724316448926160 ) ) ;
#15608 = VERTEX_POINT ( 'NONE', #6917 ) ;
#15609 = DIRECTION ( 'NONE',  ( -0.2126763768167770630, -0.9770888199431673193, 0.008136134595576584305 ) ) ;
#15610 = DIRECTION ( 'NONE',  ( 2.025474946048326158E-22, -1.000000000000000000, 1.876735158486679638E-22 ) ) ;
#15611 = CARTESIAN_POINT ( 'NONE',  ( -41.56623493000981284, 91.17157287525390075, -82.46967996629571473 ) ) ;
#15612 = ORIENTED_EDGE ( 'NONE', *, *, #8417, .F. ) ;
#15613 = CARTESIAN_POINT ( 'NONE',  ( 109.9283388797386039, 75.00188554563108312, -6.129144436280934194 ) ) ;
#15615 = CARTESIAN_POINT ( 'NONE',  ( 45.73105848731719192, 168.8134312302534283, 56.26981079935081453 ) ) ;
#15614 = DIRECTION ( 'NONE',  ( 0.9909299940865190504, -0.1338359446631136318, -0.01207007604876911971 ) ) ;
#15616 = ORIENTED_EDGE ( 'NONE', *, *, #16352, .F. ) ;
#15617 = DIRECTION ( 'NONE',  ( -0.9232306267972765212, 0.000000000000000000, 0.3842462878721248920 ) ) ;
#15618 = ORIENTED_EDGE ( 'NONE', *, *, #5826, .T. ) ;
#15619 = B_SPLINE_CURVE_WITH_KNOTS ( 'NONE', 3,
 ( #18483, #22121, #11251, #21888, #6184, #16772, #13210, #18159, #9398, #16436, #1019, #8013, #15047, #11591, #18586, #17002 ),
 .UNSPECIFIED., .F., .F.,
 ( 4, 2, 2, 2, 2, 2, 2, 4 ),
 ( 0.000000000000000000, 0.0004729024035692847407, 0.0009458048071385694814, 0.001891609614277118797, 0.002364512017846376758, 0.002837414421415635369, 0.003310316824984893113, 0.003783219228554151724 ),
 .UNSPECIFIED. ) ;
#15620 = CARTESIAN_POINT ( 'NONE',  ( -91.86813470756435152, 77.17527876199571324, 31.26628371047689114 ) ) ;
#15621 = DIRECTION ( 'NONE',  ( -7.125109674161246868E-05, 0.9999848031710253382, -0.005512562950850155054 ) ) ;
#15622 = CARTESIAN_POINT ( 'NONE',  ( 20.55752130627328000, 182.0093730182867944, 312.8173236010051141 ) ) ;
#15623 = CARTESIAN_POINT ( 'NONE',  ( -1.163172771417702700, 81.99999999999998579, -89.99248318111824574 ) ) ;
#15624 = LINE ( 'NONE', #8356, #6220 ) ;
#15625 = LINE ( 'NONE', #10443, #5944 ) ;
#15626 = ITEM_DEFINED_TRANSFORMATION ( 'NONE', 'NONE', #10290,  #6292 ) ;
#15627 = DIRECTION ( 'NONE',  ( 0.9999164797902015955, 6.965998958219364448E-18, -0.01292414190464157182 ) ) ;
#15628 = CARTESIAN_POINT ( 'NONE',  ( -3.394716948004860235, 173.8043418968527192, 324.3209156142289658 ) ) ;
#15629 = ORIENTED_EDGE ( 'NONE', *, *, #17226, .F. ) ;
#15630 = CARTESIAN_POINT ( 'NONE',  ( -48.58779557229291157, 108.9763022502714591, -43.53992698188888255 ) ) ;
#15631 = DIRECTION ( 'NONE',  ( -0.9999164797902015955, -6.965998958219364448E-18, 0.01292414190464157182 ) ) ;
#15632 = EDGE_CURVE ( 'NONE', #15758, #6141, #19803, .T. ) ;
#15633 = CARTESIAN_POINT ( 'NONE',  ( 44.31759907479521132, 171.6105373975396162, -53.08687767741515984 ) ) ;
#15634 = SHAPE_REPRESENTATION ( 'Turntable Bolt', ( #6292 ), #20590 ) ;
#15635 = DIRECTION ( 'NONE',  ( -0.01292414190463827932, 0.000000000000000000, -0.9999164797902018176 ) ) ;
#15636 = VERTEX_POINT ( 'NONE', #12562 ) ;
#15637 = EDGE_LOOP ( 'NONE', ( #18130, #3241, #4127, #14362 ) ) ;
#15638 = CARTESIAN_POINT ( 'NONE',  ( -4.705417692162559895, 172.6766985167115820, 324.0106643627350422 ) ) ;
#15639 = PRODUCT_DEFINITION_SHAPE ( 'NONE', 'NONE',  #22683 ) ;
#15640 = DIRECTION ( 'NONE',  ( 0.9999164797902015955, 2.175835928943913463E-15, -0.01292414190464156835 ) ) ;
#15641 = VERTEX_POINT ( 'NONE', #20931 ) ;
#15642 = CARTESIAN_POINT ( 'NONE',  ( -90.17429160712920577, 87.12561655205337274, 51.32195360449069454 ) ) ;
#15643 = ORIENTED_EDGE ( 'NONE', *, *, #16400, .F. ) ;
#15644 = CARTESIAN_POINT ( 'NONE',  ( 79.99331838321614896, 55.00000000000000000, -1.033931352371314949 ) ) ;
#15645 = CYLINDRICAL_SURFACE ( 'NONE', #2737, 7.500000000000002665 ) ;
#15646 = DIRECTION ( 'NONE',  ( 0.9999164797902017066, 2.457127383503899093E-15, -0.01292414190464056742 ) ) ;
#15647 = CARTESIAN_POINT ( 'NONE',  ( 13.44840881021241152, 159.0401032888326824, 299.5149227183727589 ) ) ;
#15648 = DIRECTION ( 'NONE',  ( -0.01292394549866736179, -0.005513023399721110954, -0.9999012842304692006 ) ) ;
#15649 = CYLINDRICAL_SURFACE ( 'NONE', #18889, 3.399999999999986144 ) ;
#15650 = ORIENTED_EDGE ( 'NONE', *, *, #11972, .T. ) ;
#15651 = PRODUCT_DEFINITION ( 'UNKNOWN', '', #20914, #17543 ) ;
#15652 = CARTESIAN_POINT ( 'NONE',  ( 19.10689234852680585, 168.4757078209644021, 319.8485184630963545 ) ) ;
#15653 = ORIENTED_EDGE ( 'NONE', *, *, #9034, .F. ) ;
#15654 = CARTESIAN_POINT ( 'NONE',  ( 0.000000000000000000, 37.00000000000000711, -101.0000000000000000 ) ) ;
#15655 = CARTESIAN_POINT ( 'NONE',  ( -88.16850593027358229, 88.67837445433117693, 52.45524994280101794 ) ) ;
#15656 = PRODUCT_DEFINITION_SHAPE ( 'NONE', 'NONE',  #5782 ) ;
#15657 = CARTESIAN_POINT ( 'NONE',  ( 38.69757710431291287, 94.02752048664899576, 82.47923521851859618 ) ) ;
#15658 = ORIENTED_EDGE ( 'NONE', *, *, #6553, .F. ) ;
#15659 = VERTEX_POINT ( 'NONE', #19323 ) ;
#15660 = FACE_OUTER_BOUND ( 'NONE', #10905, .T. ) ;
#15661 = CARTESIAN_POINT ( 'NONE',  ( 0.000000000000000000, 20.00000000000000000, -120.0000000000000000 ) ) ;
#15662 = PLANE ( 'NONE',  #2524 ) ;
#15663 = SURFACE_STYLE_USAGE ( .BOTH. , #11870 ) ;
#15664 = EDGE_CURVE ( 'NONE', #11011, #7441, #4668, .T. ) ;
#15665 = CARTESIAN_POINT ( 'NONE',  ( 84.85446586230914079, 75.01367125662450519, 0.5443301088886967065 ) ) ;
#15666 = DIRECTION ( 'NONE',  ( 7.125109674160258889E-05, -0.9999848031710253382, 0.005512562950849898315 ) ) ;
#15667 = ORIENTED_EDGE ( 'NONE', *, *, #496, .F. ) ;
#15668 = VERTEX_POINT ( 'NONE', #2443 ) ;
#15669 = CARTESIAN_POINT ( 'NONE',  ( -14.69408975183343635, 177.5566041281049081, 101.1392099583886051 ) ) ;
#15670 = SPHERICAL_SURFACE ( 'NONE', #7855, 2.000000000000000000 ) ;
#15671 = CARTESIAN_POINT ( 'NONE',  ( 89.24856274066357287, 79.52628152566916242, -30.13108863562650797 ) ) ;
#15672 = CARTESIAN_POINT ( 'NONE',  ( -10.90182437831279572, 114.0756104610767920, 122.8534000322088247 ) ) ;
#15673 = DIRECTION ( 'NONE',  ( 0.1296504907605110779, 0.005475273188902231650, 0.9915446392518419971 ) ) ;
#15674 = ORIENTED_EDGE ( 'NONE', *, *, #13685, .T. ) ;
#15675 = DIRECTION ( 'NONE',  ( 1.000000000000000000, 0.000000000000000000, 0.000000000000000000 ) ) ;
#15676 = DIRECTION ( 'NONE',  ( -0.01220060921879500583, -0.3298969072164960048, -0.9439381207174976085 ) ) ;
#15677 = DIRECTION ( 'NONE',  ( 0.01292414190465215537, 0.000000000000000000, 0.9999164797902015955 ) ) ;
#15678 = EDGE_CURVE ( 'NONE', #7828, #9625, #9984, .T. ) ;
#15679 = FACE_OUTER_BOUND ( 'NONE', #3613, .T. ) ;
#15680 = ORIENTED_EDGE ( 'NONE', *, *, #16427, .T. ) ;
#15681 = ORIENTED_EDGE ( 'NONE', *, *, #11458, .T. ) ;
#15682 = EDGE_LOOP ( 'NONE', ( #5633, #3790 ) ) ;
#15683 = CARTESIAN_POINT ( 'NONE',  ( -90.04173173188732449, 70.04085162602899572, 63.25014728254400609 ) ) ;
#15684 = EDGE_CURVE ( 'NONE', #979, #9760, #5881, .T. ) ;
#15685 = ORIENTED_EDGE ( 'NONE', *, *, #2177, .T. ) ;
#15686 = CARTESIAN_POINT ( 'NONE',  ( -91.21019055468684655, 34.61572286322119396, -28.82359390673209631 ) ) ;
#15687 = CARTESIAN_POINT ( 'NONE',  ( -90.10167664437891233, 70.10962226922626428, 63.10072484710806151 ) ) ;
#15688 = ADVANCED_FACE ( 'NONE', ( #7497 ), #12686, .T. ) ;
#15689 = DIRECTION ( 'NONE',  ( -0.9934404589540162256, -0.1135548637187056842, 0.01346653032743081423 ) ) ;
#15690 = CARTESIAN_POINT ( 'NONE',  ( -40.94813932551374336, 95.97017003981163441, 82.42564028881615457 ) ) ;
#15691 = EDGE_CURVE ( 'NONE', #16093, #10046, #3922, .T. ) ;
#15692 = ORIENTED_EDGE ( 'NONE', *, *, #18593, .F. ) ;
#15693 =( NAMED_UNIT ( * ) SI_UNIT ( $, .STERADIAN. ) SOLID_ANGLE_UNIT ( ) );
#15694 = CARTESIAN_POINT ( 'NONE',  ( 153.9999999999992610, 1.999999999999998224, -53.76161406891471017 ) ) ;
#15695 = CARTESIAN_POINT ( 'NONE',  ( 11.76425125167022578, 187.8086852021691016, 307.7642755247033506 ) ) ;
#15696 = CARTESIAN_POINT ( 'NONE',  ( -51.70139581094897352, 189.5987791479411442, -72.16877407953693080 ) ) ;
#15697 = CARTESIAN_POINT ( 'NONE',  ( 90.46145803316728973, 80.27058204906826688, -32.37524683357428046 ) ) ;
#15698 = ORIENTED_EDGE ( 'NONE', *, *, #22096, .T. ) ;
#15699 = AXIS2_PLACEMENT_3D ( 'NONE', #18998, #15479, #13846 ) ;
#15700 = EDGE_CURVE ( 'NONE', #10176, #21136, #6043, .T. ) ;
#15701 = CARTESIAN_POINT ( 'NONE',  ( -12.81536461602102683, 326.2504838843369726, 414.3222871145668478 ) ) ;
#15702 = CARTESIAN_POINT ( 'NONE',  ( -8.195910149518317311, 185.6194122973667788, 308.0197546130458477 ) ) ;
#15703 = ORIENTED_EDGE ( 'NONE', *, *, #16113, .F. ) ;
#15704 = ADVANCED_FACE ( 'NONE', ( #14757 ), #11767, .T. ) ;
#15705 = CARTESIAN_POINT ( 'NONE',  ( -2.096375399687082197, 190.2200455327031534, 274.6112675210154634 ) ) ;
#15706 = ORIENTED_EDGE ( 'NONE', *, *, #1876, .F. ) ;
#15707 = B_SPLINE_CURVE_WITH_KNOTS ( 'NONE', 3,
 ( #13901, #14027, #22482, #1506 ),
 .UNSPECIFIED., .F., .F.,
 ( 4, 4 ),
 ( 0.1567379737884350976, 0.1627913398252618382 ),
 .UNSPECIFIED. ) ;
#15708 = EDGE_CURVE ( 'NONE', #13344, #16500, #12137, .T. ) ;
#15709 = CARTESIAN_POINT ( 'NONE',  ( -70.71197882986197669, 71.18508886668922742, -84.26048200481868378 ) ) ;
#15710 = DIRECTION ( 'NONE',  ( 7.125109674364534776E-05, -0.9999848031710252272, 0.005512562950849704893 ) ) ;
#15711 = UNCERTAINTY_MEASURE_WITH_UNIT (LENGTH_MEASURE( 1.000000000000000082E-05 ), #16234, 'distance_accuracy_value', 'NONE');
#15712 = ORIENTED_EDGE ( 'NONE', *, *, #2286, .T. ) ;
#15713 = DIRECTION ( 'NONE',  ( -0.000000000000000000, -1.000000000000000000, -0.000000000000000000 ) ) ;
#15715 = VECTOR ( 'NONE', #20549, 1000.000000000000114 ) ;
#15714 =( LENGTH_UNIT ( ) NAMED_UNIT ( * ) SI_UNIT ( .MILLI., .METRE. ) );
#15716 = CARTESIAN_POINT ( 'NONE',  ( 19.85977264408844079, 148.5551973574642943, 278.3773732832850101 ) ) ;
#15717 = ADVANCED_FACE ( 'NONE', ( #18291 ), #377, .F. ) ;
#15718 = ORIENTED_EDGE ( 'NONE', *, *, #21561, .T. ) ;
#15719 = CARTESIAN_POINT ( 'NONE',  ( 12.99862026951066518, 190.3184116425491368, 320.8540507871223326 ) ) ;
#15720 = ORIENTED_EDGE ( 'NONE', *, *, #1131, .T. ) ;
#15721 = ORIENTED_EDGE ( 'NONE', *, *, #6401, .T. ) ;
#15722 = DIRECTION ( 'NONE',  ( -7.125109674243555432E-05, 0.9999848031710253382, -0.005512562950850175003 ) ) ;
#15723 = DIRECTION ( 'NONE',  ( -0.01292394549866632963, -0.005513023399716958026, -0.9999012842304692006 ) ) ;
#15724 = CARTESIAN_POINT ( 'NONE',  ( 18.27202492469069028, 422.9831327814429756, 371.0727646550985241 ) ) ;
#15725 = PRESENTATION_STYLE_ASSIGNMENT (( #8675 ) ) ;
#15726 = ORIENTED_EDGE ( 'NONE', *, *, #5154, .F. ) ;
#15727 = VECTOR ( 'NONE', #7842, 1000.000000000000114 ) ;
#15728 = CARTESIAN_POINT ( 'NONE',  ( -41.00000899811524846, 169.5540992312279229, 273.1580453575298293 ) ) ;
#15729 = CARTESIAN_POINT ( 'NONE',  ( 0.000000000000000000, 37.00000000000000711, 0.000000000000000000 ) ) ;
#15730 = DIRECTION ( 'NONE',  ( 0.009138748381789078140, -0.7071067811865487940, 0.7070477234798315802 ) ) ;
#15731 = DIRECTION ( 'NONE',  ( -0.000000000000000000, -1.000000000000000000, -0.000000000000000000 ) ) ;
#15732 = B_SPLINE_CURVE_WITH_KNOTS ( 'NONE', 3,
 ( #3076, #15283, #2848, #13541, #9859, #2957 ),
 .UNSPECIFIED., .F., .F.,
 ( 4, 2, 4 ),
 ( 0.01452727543195645593, 0.01715716534226980824, 0.01978705525258316056 ),
 .UNSPECIFIED. ) ;
#15733 = COLOUR_RGB ( '', 0.66274510, 0.83137255, 0.94901961) ;
#15734 = CARTESIAN_POINT ( 'NONE',  ( 20.66284806145036157, 181.9102389805751159, 313.6090225492346804 ) ) ;
#15735 = ADVANCED_FACE ( 'NONE', ( #12908 ), #7371, .T. ) ;
#15736 = PLANE ( 'NONE',  #11177 ) ;
#15737 = DIRECTION ( 'NONE',  ( 0.009371490965938892789, 0.6886276452575282869, 0.7250545781830131098 ) ) ;
#15738 = DIRECTION ( 'NONE',  ( 0.9909299940865187173, -0.1338359446631179062, -0.01207007604876208194 ) ) ;
#15739 = DIRECTION ( 'NONE',  ( 0.9909299940865187173, -0.1338359446631179062, -0.01207007604876208194 ) ) ;
#15740 = CARTESIAN_POINT ( 'NONE',  ( 158.3970384574715808, 20.00000000000000000, 62.74304228515676130 ) ) ;
#15741 = VECTOR ( 'NONE', #22057, 1000.000000000000114 ) ;
#15742 = CARTESIAN_POINT ( 'NONE',  ( 14.19652144490156687, 105.7231500355213853, 131.1758847094702389 ) ) ;
#15743 = EDGE_CURVE ( 'NONE', #10523, #9499, #2463, .T. ) ;
#15744 = LINE ( 'NONE', #6763, #14471 ) ;
#15745 = DIRECTION ( 'NONE',  ( -7.125109674158749138E-05, 0.9999848031710253382, -0.005512562950850162860 ) ) ;
#15746 = CIRCLE ( 'NONE', #11341, 24.99999999999998224 ) ;
#15747 = CARTESIAN_POINT ( 'NONE',  ( -44.75576560912451640, 168.6025580852140706, 19.18675944895310082 ) ) ;
#15748 = ORIENTED_EDGE ( 'NONE', *, *, #7659, .F. ) ;
#15749 = CARTESIAN_POINT ( 'NONE',  ( 7.825680009415360239, 81.92243737533797798, -91.81739557479740199 ) ) ;
#15750 = LINE ( 'NONE', #13793, #19934 ) ;
#15751 = ORIENTED_EDGE ( 'NONE', *, *, #16400, .T. ) ;
#15752 = CARTESIAN_POINT ( 'NONE',  ( 49.73769616939263472, 110.3486766201082503, -47.52380993751345528 ) ) ;
#15753 = ORIENTED_EDGE ( 'NONE', *, *, #3283, .T. ) ;
#15754 = DIRECTION ( 'NONE',  ( 7.125109674161259066E-05, -0.9999848031710252272, 0.005512562950850163727 ) ) ;
#15755 = DIRECTION ( 'NONE',  ( 0.006595249899610063603, 0.8599936914359664897, 0.5102620438256224578 ) ) ;
#15756 = PLANE ( 'NONE',  #15348 ) ;
#15757 = DIRECTION ( 'NONE',  ( -0.7098319280015157329, 0.09073800780701535285, -0.6985021459729847670 ) ) ;
#15758 = VERTEX_POINT ( 'NONE', #10320 ) ;
#15759 = CARTESIAN_POINT ( 'NONE',  ( 153.9999999999992610, 18.00000000000000355, -53.76161406891471017 ) ) ;
#15760 = LINE ( 'NONE', #4, #17830 ) ;
#15761 = CIRCLE ( 'NONE', #10970, 83.99999999999998579 ) ;
#15762 = ORIENTED_EDGE ( 'NONE', *, *, #8656, .F. ) ;
#15763 = CARTESIAN_POINT ( 'NONE',  ( -1.710339879361044035, 327.0957934528446458, 309.0913701133406448 ) ) ;
#15764 = EDGE_CURVE ( 'NONE', #6123, #5251, #17643, .T. ) ;
#15765 = ADVANCED_FACE ( 'NONE', ( #17209 ), #5125, .F. ) ;
#15766 = AXIS2_PLACEMENT_3D ( 'NONE', #22348, #1598, #22464 ) ;
#15767 = EDGE_LOOP ( 'NONE', ( #17638, #8625 ) ) ;
#15768 = CARTESIAN_POINT ( 'NONE',  ( 90.73535795930332881, 70.47419434645436809, -62.18621042075483984 ) ) ;
#15769 = CARTESIAN_POINT ( 'NONE',  ( -89.58129464662867747, 89.08235497554598226, 51.76997070739610507 ) ) ;
#15770 = SHAPE_REPRESENTATION ( 'Hex Nut', ( #6292 ), #7391 ) ;
#15771 = FACE_OUTER_BOUND ( 'NONE', #6000, .T. ) ;
#15772 = ORIENTED_EDGE ( 'NONE', *, *, #8901, .T. ) ;
#15773 = VERTEX_POINT ( 'NONE', #1591 ) ;
#15774 = DIRECTION ( 'NONE',  ( -0.009188991635465687535, 0.7031977391749432149, -0.7109349492407668336 ) ) ;
#15775 = CARTESIAN_POINT ( 'NONE',  ( 161.9999999999992610, 0.000000000000000000, -53.76161406891482386 ) ) ;
#15776 = CARTESIAN_POINT ( 'NONE',  ( -69.43142427201328815, 92.58578643762699301, 85.31868097644080251 ) ) ;
#15777 = AXIS2_PLACEMENT_3D ( 'NONE', #19806, #16640, #543 ) ;
#15778 = CARTESIAN_POINT ( 'NONE',  ( 82.31124572168572229, 75.11021523748625839, 3.511968633515443194 ) ) ;
#15779 = CIRCLE ( 'NONE', #8059, 10.29357798165139393 ) ;
#15780 = DIRECTION ( 'NONE',  ( 1.000000000000000000, 0.000000000000000000, -1.386679829960243376E-14 ) ) ;
#15781 = ORIENTED_EDGE ( 'NONE', *, *, #18112, .F. ) ;
#15782 = ORIENTED_EDGE ( 'NONE', *, *, #13327, .F. ) ;
#15783 = VECTOR ( 'NONE', #20868, 1000.000000000000114 ) ;
#15784 = CARTESIAN_POINT ( 'NONE',  ( 1.421655609510571683, 55.00000000000000000, 109.9908127769221551 ) ) ;
#15785 = CARTESIAN_POINT ( 'NONE',  ( -76.10506960740103466, 75.05939835648032954, 4.351290691204203753 ) ) ;
#15786 = CARTESIAN_POINT ( 'NONE',  ( -10.97446589277025808, 164.9932245799013799, 309.3419758684869976 ) ) ;
#15787 = PLANE ( 'NONE',  #18734 ) ;
#15788 = EDGE_LOOP ( 'NONE', ( #9683, #857, #8121, #2182 ) ) ;
#15789 = CARTESIAN_POINT ( 'NONE',  ( -37.74321565662646805, 93.98903676387503481, -82.45639044149366725 ) ) ;
#15790 = CARTESIAN_POINT ( 'NONE',  ( 48.31072223536580879, 166.8507685304811048, 256.0170097695140043 ) ) ;
#15791 = CARTESIAN_POINT ( 'NONE',  ( 105.0182314695230872, 70.09775045434527385, -32.72898861654378067 ) ) ;
#15792 = ORIENTED_EDGE ( 'NONE', *, *, #12866, .F. ) ;
#15793 = EDGE_CURVE ( 'NONE', #15219, #6576, #9730, .T. ) ;
#15794 = CYLINDRICAL_SURFACE ( 'NONE', #15131, 2.499999999999988010 ) ;
#15795 = ORIENTED_EDGE ( 'NONE', *, *, #8937, .T. ) ;
#15796 = VERTEX_POINT ( 'NONE', #1481 ) ;
#15797 = CIRCLE ( 'NONE', #10999, 2.000000000000001332 ) ;
#15798 = VERTEX_POINT ( 'NONE', #13775 ) ;
#15799 = AXIS2_PLACEMENT_3D ( 'NONE', #9787, #17032, #13362 ) ;
#15800 = CARTESIAN_POINT ( 'NONE',  ( 16.22504546523506264, 187.9132589410656919, 308.8173052943575954 ) ) ;
#15802 = ORIENTED_EDGE ( 'NONE', *, *, #16282, .F. ) ;
#15801 = EDGE_LOOP ( 'NONE', ( #21143, #4372, #21892, #15188, #16713, #17249, #1750, #9010, #7570, #4226 ) ) ;
#15803 = AXIS2_PLACEMENT_3D ( 'NONE', #20282, #18240, #9840 ) ;
#15804 = LINE ( 'NONE', #12355, #3607 ) ;
#15805 = CARTESIAN_POINT ( 'NONE',  ( 1.364375150383346228E-14, 45.00000000000000000, -9.836439021161248541E-15 ) ) ;
#15806 = CARTESIAN_POINT ( 'NONE',  ( -1.893392603924682671, 142.7666083241327328, 274.9837640348721379 ) ) ;
#15807 = PLANE ( 'NONE',  #22477 ) ;
#15808 = EDGE_CURVE ( 'NONE', #19674, #8677, #7726, .T. ) ;
#15809 = DIRECTION ( 'NONE',  ( -0.8981428216242087759, 0.000000000000000000, 0.4397038457472309259 ) ) ;
#15810 = CARTESIAN_POINT ( 'NONE',  ( 83.74446663462045137, 75.12966630363247589, -6.049935108198452482 ) ) ;
#15811 = CARTESIAN_POINT ( 'NONE',  ( 17.35553945970433887, 186.7678997353801549, 309.5505051628369415 ) ) ;
#15812 = PLANE ( 'NONE',  #14872 ) ;
#15813 = VECTOR ( 'NONE', #11991, 999.9999999999998863 ) ;
#15814 = AXIS2_PLACEMENT_3D ( 'NONE', #13939, #5530, #5189 ) ;
#15815 = DIRECTION ( 'NONE',  ( -0.01292394549866632963, -0.005513023399716958026, -0.9999012842304692006 ) ) ;
#15816 = VECTOR ( 'NONE', #17463, 1000.000000000000000 ) ;
#15817 = AXIS2_PLACEMENT_3D ( 'NONE', #20813, #17398, #19092 ) ;
#15818 = SPHERICAL_SURFACE ( 'NONE', #8811, 2.000000000000000000 ) ;
#15819 = CIRCLE ( 'NONE', #20172, 117.0000000000000000 ) ;
#15820 = CARTESIAN_POINT ( 'NONE',  ( -35.42010074854528767, 108.0982075334647163, 199.8475074598744072 ) ) ;
#15821 = ORIENTED_EDGE ( 'NONE', *, *, #2370, .F. ) ;
#15822 = CARTESIAN_POINT ( 'NONE',  ( -91.96840972750146648, 79.95771593962433599, -29.13399816620382055 ) ) ;
#15823 = EDGE_CURVE ( 'NONE', #17283, #7401, #3533, .T. ) ;
#15824 = VERTEX_POINT ( 'NONE', #1273 ) ;
#15825 = ADVANCED_FACE ( 'NONE', ( #8260 ), #18818, .T. ) ;
#15826 = VECTOR ( 'NONE', #16882, 1000.000000000000000 ) ;
#15827 = PRODUCT_DEFINITION_SHAPE ( 'NONE', 'NONE',  #22676 ) ;
#15828 = AXIS2_PLACEMENT_3D ( 'NONE', #4759, #11802, #8437 ) ;
#15829 = DIRECTION ( 'NONE',  ( 0.01292414190464131335, 1.902755938799530239E-22, 0.9999164797902015955 ) ) ;
#15830 = AXIS2_PLACEMENT_3D ( 'NONE', #20883, #3542, #1824 ) ;
#15831 = DIRECTION ( 'NONE',  ( 0.01292394549866738608, 0.005513023399720468239, 0.9999012842304692006 ) ) ;
#15832 = DIRECTION ( 'NONE',  ( -0.01292414190463827932, 0.000000000000000000, -0.9999164797902018176 ) ) ;
#15833 = EDGE_CURVE ( 'NONE', #22352, #12132, #14000, .T. ) ;
#15834 = DIRECTION ( 'NONE',  ( -2.025474946048326393E-22, 1.000000000000000000, -1.876735158486679873E-22 ) ) ;
#15835 = AXIS2_PLACEMENT_3D ( 'NONE', #16392, #2702, #6377 ) ;
#15836 = EDGE_LOOP ( 'NONE', ( #3902, #8414, #22169, #293 ) ) ;
#15837 = EDGE_CURVE ( 'NONE', #9818, #17159, #12041, .T. ) ;
#15838 = LINE ( 'NONE', #22661, #18314 ) ;
#15839 = ORIENTED_EDGE ( 'NONE', *, *, #2852, .T. ) ;
#15840 = CARTESIAN_POINT ( 'NONE',  ( -41.99143391042890272, 165.8447256859541596, 232.8944075815348924 ) ) ;
#15841 = EDGE_CURVE ( 'NONE', #2746, #21650, #22564, .T. ) ;
#15842 = CARTESIAN_POINT ( 'NONE',  ( 5.178247477726851677, 158.1956793026589025, 324.6289403114667493 ) ) ;
#15843 = ORIENTED_EDGE ( 'NONE', *, *, #8503, .T. ) ;
#15844 = CARTESIAN_POINT ( 'NONE',  ( -10.38911361869056904, 187.1603952044747814, 321.0948210509291130 ) ) ;
#15845 = CARTESIAN_POINT ( 'NONE',  ( 79.99331838321626265, 54.99999999999999289, -1.033931352371318058 ) ) ;
#15846 = DIRECTION ( 'NONE',  ( 7.125109674403277385E-05, -0.9999848031710253382, 0.005512562950848281552 ) ) ;
#15847 = EDGE_LOOP ( 'NONE', ( #2505, #6492, #12786, #10649 ) ) ;
#15848 = CARTESIAN_POINT ( 'NONE',  ( -14.17380171632341224, 184.4915598789741011, 322.7338882641075770 ) ) ;
#15849 = AXIS2_PLACEMENT_3D ( 'NONE', #9462, #16497, #11313 ) ;
#15850 = ORIENTED_EDGE ( 'NONE', *, *, #7665, .T. ) ;
#15851 = PRODUCT ( 'Turntable Bolt', 'Turntable Bolt', '', ( #16451 ) ) ;
#15852 = CARTESIAN_POINT ( 'NONE',  ( -10.95317072096182187, 113.6585260871128611, 119.7560427279830009 ) ) ;
#15853 = CARTESIAN_POINT ( 'NONE',  ( -83.58290648752343088, 104.4142135623730780, -71.51152175067954886 ) ) ;
#15854 = CARTESIAN_POINT ( 'NONE',  ( -14.58871019898540489, 179.2506784104788835, 319.3598715905317249 ) ) ;
#15855 = EDGE_CURVE ( 'NONE', #22544, #11891, #13546, .T. ) ;
#15856 = CARTESIAN_POINT ( 'NONE',  ( -91.62437796271721879, 95.44063823554751025, -60.86849236629028326 ) ) ;
#15857 = EDGE_CURVE ( 'NONE', #7115, #11923, #9567, .T. ) ;
#15858 = CIRCLE ( 'NONE', #8129, 2.000000000000008438 ) ;
#15859 = DIRECTION ( 'NONE',  ( -0.01292394549866727679, -0.005513023399720743192, -0.9999012842304693116 ) ) ;
#15860 = CARTESIAN_POINT ( 'NONE',  ( 0.000000000000000000, 20.00000000000000000, -126.0000000000000000 ) ) ;
#15861 = CONTEXT_DEPENDENT_SHAPE_REPRESENTATION ( #18528, #19283 ) ;
#15862 = VECTOR ( 'NONE', #21348, 1000.000000000000227 ) ;
#15863 = AXIS2_PLACEMENT_3D ( 'NONE', #1141, #2410, #22003 ) ;
#15864 = DIRECTION ( 'NONE',  ( -0.9999164797902015955, -6.965998958219364448E-18, 0.01292414190464157182 ) ) ;
#15865 = CARTESIAN_POINT ( 'NONE',  ( -38.27775742616200461, 165.9786531560170033, 257.1409935088582870 ) ) ;
#15866 = DIRECTION ( 'NONE',  ( -0.9999164797902017066, 0.000000000000000000, 0.01292414190463832269 ) ) ;
#15867 = DIRECTION ( 'NONE',  ( 0.9999164797902017066, 0.000000000000000000, -0.01292414190464174703 ) ) ;
#15868 = ORIENTED_EDGE ( 'NONE', *, *, #20841, .T. ) ;
#15869 = PLANE ( 'NONE',  #1337 ) ;
#15870 = DIRECTION ( 'NONE',  ( -2.025474946048326158E-22, 1.000000000000000000, -1.876735158486679638E-22 ) ) ;
#15871 = ORIENTED_EDGE ( 'NONE', *, *, #21536, .T. ) ;
#15872 = EDGE_CURVE ( 'NONE', #6677, #3377, #13666, .T. ) ;
#15873 = CARTESIAN_POINT ( 'NONE',  ( 49.97797887564394870, 113.1447607658756880, -44.83689451937377868 ) ) ;
#15874 = AXIS2_PLACEMENT_3D ( 'NONE', #18299, #18634, #9909 ) ;
#15875 = EDGE_LOOP ( 'NONE', ( #22197, #22019, #758, #20580 ) ) ;
#15876 = LINE ( 'NONE', #21127, #6029 ) ;
#15877 = DIRECTION ( 'NONE',  ( 0.000000000000000000, -1.000000000000000000, 0.000000000000000000 ) ) ;
#15878 = DIRECTION ( 'NONE',  ( -0.01292414190464224663, 0.000000000000000000, -0.9999164797902015955 ) ) ;
#15879 = ORIENTED_EDGE ( 'NONE', *, *, #5675, .F. ) ;
#15880 = ORIENTED_EDGE ( 'NONE', *, *, #18021, .F. ) ;
#15881 = FACE_OUTER_BOUND ( 'NONE', #17612, .T. ) ;
#15882 = CARTESIAN_POINT ( 'NONE',  ( 0.000000000000000000, 29.00000000000000355, 0.000000000000000000 ) ) ;
#15883 = AXIS2_PLACEMENT_3D ( 'NONE', #15578, #22084, #13842 ) ;
#15884 = VECTOR ( 'NONE', #3740, 1000.000000000000114 ) ;
#15885 = AXIS2_PLACEMENT_3D ( 'NONE', #4714, #5683, #419 ) ;
#15886 = EDGE_CURVE ( 'NONE', #17969, #9954, #6994, .T. ) ;
#15887 = EDGE_LOOP ( 'NONE', ( #5352, #581 ) ) ;
#15888 = DIRECTION ( 'NONE',  ( -0.01292414190463827932, 0.000000000000000000, -0.9999164797902018176 ) ) ;
#15889 = CARTESIAN_POINT ( 'NONE',  ( -88.16677217749351314, 88.55790908203320555, 52.61947244965261916 ) ) ;
#15890 = AXIS2_PLACEMENT_3D ( 'NONE', #12179, #17351, #13894 ) ;
#15892 = VERTEX_POINT ( 'NONE', #14742 ) ;
#15891 = EDGE_LOOP ( 'NONE', ( #19959, #19281, #245, #11800 ) ) ;
#15893 =( REPRESENTATION_RELATIONSHIP ('NONE','NONE', #11808, #19567 ) REPRESENTATION_RELATIONSHIP_WITH_TRANSFORMATION ( #16428 )SHAPE_REPRESENTATION_RELATIONSHIP( ) );
#15894 = ORIENTED_EDGE ( 'NONE', *, *, #7131, .F. ) ;
#15895 = DIRECTION ( 'NONE',  ( -0.3101392564284290998, -0.9506461370142487155, 0.009250070373107117244 ) ) ;
#15896 = CARTESIAN_POINT ( 'NONE',  ( -10.89482230603750246, 73.92842581583312267, 123.4747019167147499 ) ) ;
#15897 = AXIS2_PLACEMENT_3D ( 'NONE', #17194, #13865, #1469 ) ;
#15898 = CARTESIAN_POINT ( 'NONE',  ( -4.397794363141794172, 165.8073523762867012, 324.7117453967128995 ) ) ;
#15899 = DIRECTION ( 'NONE',  ( -0.01292394549866632963, -0.005513023399716958026, -0.9999012842304692006 ) ) ;
#15900 = ORIENTED_EDGE ( 'NONE', *, *, #1223, .F. ) ;
#15901 = ADVANCED_FACE ( 'NONE', ( #20987 ), #4997, .F. ) ;
#15902 = CARTESIAN_POINT ( 'NONE',  ( 13.87343267002348846, 188.5565630873763325, 276.5910899882047147 ) ) ;
#15903 = ORIENTED_EDGE ( 'NONE', *, *, #4152, .F. ) ;
#15904 = CARTESIAN_POINT ( 'NONE',  ( 47.42524840967396216, 108.3817487785542824, -44.77763872393808953 ) ) ;
#15905 = EDGE_CURVE ( 'NONE', #5251, #14784, #22321, .T. ) ;
#15906 = CARTESIAN_POINT ( 'NONE',  ( -16.55822128367782753, 177.6144908738019694, 111.6640217266178041 ) ) ;
#15907 = CARTESIAN_POINT ( 'NONE',  ( -77.79076858216454582, 75.11053174630313833, -3.578068059858031447 ) ) ;
#15908 = CARTESIAN_POINT ( 'NONE',  ( -28.49296332856286185, 324.0493105597922749, 313.1455847166214426 ) ) ;
#15909 = ORIENTED_EDGE ( 'NONE', *, *, #682, .T. ) ;
#15910 = FACE_OUTER_BOUND ( 'NONE', #21657, .T. ) ;
#15911 = ORIENTED_EDGE ( 'NONE', *, *, #12235, .F. ) ;
#15912 = DIRECTION ( 'NONE',  ( 0.9232306267972774094, 0.000000000000000000, -0.3842462878721227826 ) ) ;
#15913 = DIRECTION ( 'NONE',  ( 0.009760756503427210282, -0.9999378516499566327, 0.005387065077606872227 ) ) ;
#15914 = CARTESIAN_POINT ( 'NONE',  ( 105.2250167141420150, 70.47859713728952613, -32.05784361718419717 ) ) ;
#15915 = EDGE_LOOP ( 'NONE', ( #21597, #6729, #12334, #12501 ) ) ;
#15916 = LINE ( 'NONE', #16141, #9224 ) ;
#15917 = ORIENTED_EDGE ( 'NONE', *, *, #21170, .F. ) ;
#15918 = AXIS2_PLACEMENT_3D ( 'NONE', #3253, #17175, #17416 ) ;
#15919 = ORIENTED_EDGE ( 'NONE', *, *, #15568, .T. ) ;
#15920 = ORIENTED_EDGE ( 'NONE', *, *, #13113, .F. ) ;
#15921 = VECTOR ( 'NONE', #8175, 999.9999999999998863 ) ;
#15922 = UNCERTAINTY_MEASURE_WITH_UNIT (LENGTH_MEASURE( 1.000000000000000082E-05 ), #11322, 'distance_accuracy_value', 'NONE');
#15923 = CARTESIAN_POINT ( 'NONE',  ( -10.85626963016051150, 114.0998676838791681, 127.2530973345311907 ) ) ;
#15924 = ORIENTED_EDGE ( 'NONE', *, *, #13859, .F. ) ;
#15925 = CARTESIAN_POINT ( 'NONE',  ( 3.560643301544068162, 141.4162645520002002, 256.7356493073644401 ) ) ;
#15926 = CYLINDRICAL_SURFACE ( 'NONE', #18793, 75.00000000000002842 ) ;
#15927 = CARTESIAN_POINT ( 'NONE',  ( -2.283878053185306456, 142.8671684950954841, 275.1583867193013475 ) ) ;
#15928 = CIRCLE ( 'NONE', #19204, 7.999999999999985789 ) ;
#15929 = FACE_BOUND ( 'NONE', #20629, .T. ) ;
#15930 = CARTESIAN_POINT ( 'NONE',  ( -38.77389020828243815, 95.32323862687174199, 83.05169643453594119 ) ) ;
#15931 =( LENGTH_UNIT ( ) NAMED_UNIT ( * ) SI_UNIT ( .MILLI., .METRE. ) );
#15932 = FACE_OUTER_BOUND ( 'NONE', #12601, .T. ) ;
#15933 = CARTESIAN_POINT ( 'NONE',  ( 17.07179474224462723, 187.0711841522102930, 309.3407821921324512 ) ) ;
#15934 = VECTOR ( 'NONE', #20697, 1000.000000000000114 ) ;
#15935 = CARTESIAN_POINT ( 'NONE',  ( 92.25740333815001293, 79.89798572914074271, 28.97539206162133141 ) ) ;
#15936 = CIRCLE ( 'NONE', #18126, 6.000000000000003553 ) ;
#15937 = ORIENTED_EDGE ( 'NONE', *, *, #17126, .F. ) ;
#15938 = CARTESIAN_POINT ( 'NONE',  ( -55.34016076973275489, 143.9188730675114414, 167.4742716441172377 ) ) ;
#15939 = ORIENTED_EDGE ( 'NONE', *, *, #13304, .T. ) ;
#15940 = CARTESIAN_POINT ( 'NONE',  ( 45.44350069997230435, 168.6907664596095344, 34.02200722522286469 ) ) ;
#15941 = DIRECTION ( 'NONE',  ( -0.9999164797902017066, 0.000000000000000000, 0.01292414190464157529 ) ) ;
#15942 = VERTEX_POINT ( 'NONE', #10293 ) ;
#15943 = AXIS2_PLACEMENT_3D ( 'NONE', #22403, #4956, #20809 ) ;
#15944 = B_SPLINE_CURVE_WITH_KNOTS ( 'NONE', 3,
 ( #4418, #16749, #11445, #15986, #9735, #7328, #18457 ),
 .UNSPECIFIED., .F., .F.,
 ( 4, 3, 4 ),
 ( 0.0004832953973055784786, 0.005203611832036382848, 0.01040722366698936321 ),
 .UNSPECIFIED. ) ;
#15945 = CIRCLE ( 'NONE', #4896, 7.000000000000022204 ) ;
#15946 = CARTESIAN_POINT ( 'NONE',  ( -93.13093775432008670, 79.82103140526460550, -28.79876782389536771 ) ) ;
#15947 = ORIENTED_EDGE ( 'NONE', *, *, #6703, .T. ) ;
#15948 = B_SPLINE_CURVE_WITH_KNOTS ( 'NONE', 3,
 ( #8194, #6683, #6902, #20692, #17050, #22393, #20801, #1528, #4830, #13922, #5056, #18744, #1197, #12088, #4947, #17146, #19078, #20913 ),
 .UNSPECIFIED., .F., .F.,
 ( 4, 2, 2, 2, 2, 2, 2, 2, 4 ),
 ( 0.006298532399469907589, 0.01549750422645886604, 0.02009699013995334266, 0.02239673309670057316, 0.02469647605344780367, 0.03389544788043670487, 0.03849493379393116588, 0.04079467675067838250, 0.04309441970742561301 ),
 .UNSPECIFIED. ) ;
#15949 = CONICAL_SURFACE ( 'NONE', #17783, 2.499999999999988010, 1.029744258676651425 ) ;
#15950 = AXIS2_PLACEMENT_3D ( 'NONE', #16281, #19253, #3517 ) ;
#15951 = CARTESIAN_POINT ( 'NONE',  ( 19.16736913329742009, 177.4987173824078468, 90.20082564921086998 ) ) ;
#15952 = CARTESIAN_POINT ( 'NONE',  ( -13.92525281995234820, 325.7770340667113942, 328.4523304068723064 ) ) ;
#15953 = PRODUCT_DEFINITION_CONTEXT ( 'detailed design', #1483, 'design' ) ;
#15954 = DIRECTION ( 'NONE',  ( -7.125109674403276030E-05, 0.9999848031710252272, -0.005512562950848280685 ) ) ;
#15955 = DIRECTION ( 'NONE',  ( 7.125109674403837105E-05, -0.9999848031710252272, 0.005512562950847867821 ) ) ;
#15956 = EDGE_LOOP ( 'NONE', ( #22582, #12712, #16479, #7991, #17042, #1760 ) ) ;
#15957 = CARTESIAN_POINT ( 'NONE',  ( 12.88848270841033639, 190.3578502642233445, 320.8635863820699115 ) ) ;
#15958 = ORIENTED_EDGE ( 'NONE', *, *, #8572, .F. ) ;
#15959 = CIRCLE ( 'NONE', #18860, 2.000000000000004441 ) ;
#15960 = DIRECTION ( 'NONE',  ( 7.125109674160258889E-05, -0.9999848031710252272, 0.005512562950849897447 ) ) ;
#15961 = ADVANCED_FACE ( 'NONE', ( #17186 ), #17427, .T. ) ;
#15962 = DIRECTION ( 'NONE',  ( -2.025474946048326158E-22, 1.000000000000000000, -1.876735158486679638E-22 ) ) ;
#15963 = CARTESIAN_POINT ( 'NONE',  ( 71.61338682171094661, 92.58578643762700722, 83.49564556265194426 ) ) ;
#15964 = CARTESIAN_POINT ( 'NONE',  ( -8.478337820821147730, 185.2758271473933007, 323.2502905065526875 ) ) ;
#15965 = CARTESIAN_POINT ( 'NONE',  ( -92.11140453220255608, 79.82915613195359583, 31.20677464679524604 ) ) ;
#15966 = ORIENTED_EDGE ( 'NONE', *, *, #3061, .F. ) ;
#15967 = CARTESIAN_POINT ( 'NONE',  ( -54.52327687265812983, 1.999999999999998224, 111.3697098814011923 ) ) ;
#15968 = AXIS2_PLACEMENT_3D ( 'NONE', #18555, #2366, #15127 ) ;
#15969 = ORIENTED_EDGE ( 'NONE', *, *, #4169, .T. ) ;
#15970 = CARTESIAN_POINT ( 'NONE',  ( -50.34311518839565736, 114.2252428643726319, 168.6470458426240668 ) ) ;
#15971 = DIRECTION ( 'NONE',  ( 7.125109674160258889E-05, -0.9999848031710252272, 0.005512562950849897447 ) ) ;
#15972 = CARTESIAN_POINT ( 'NONE',  ( -14.95284176865328263, 180.0521946526295949, 316.6167187968075041 ) ) ;
#15973 = CARTESIAN_POINT ( 'NONE',  ( 12.11216763350604175, 187.6476608629002385, 304.8965484581246415 ) ) ;
#15974 = EDGE_CURVE ( 'NONE', #14784, #16406, #19822, .T. ) ;
#15975 = EDGE_CURVE ( 'NONE', #16242, #5068, #15112, .T. ) ;
#15976 = VECTOR ( 'NONE', #8527, 1000.000000000000114 ) ;
#15977 = VERTEX_POINT ( 'NONE', #8235 ) ;
#15978 = CARTESIAN_POINT ( 'NONE',  ( 0.000000000000000000, 1.999999999999998224, 0.000000000000000000 ) ) ;
#15979 = EDGE_CURVE ( 'NONE', #10504, #19051, #6509, .T. ) ;
#15980 = ORIENTED_EDGE ( 'NONE', *, *, #21684, .F. ) ;
#15981 = DIRECTION ( 'NONE',  ( 1.000000000000000000, 0.000000000000000000, 0.000000000000000000 ) ) ;
#15982 = CARTESIAN_POINT ( 'NONE',  ( 80.05923150692980528, 55.00000000000000000, 4.065642694558706971 ) ) ;
#15983 = PLANE ( 'NONE',  #5592 ) ;
#15984 = EDGE_CURVE ( 'NONE', #11891, #16331, #20737, .T. ) ;
#15985 = EDGE_LOOP ( 'NONE', ( #270, #11292, #18571 ) ) ;
#15986 = CARTESIAN_POINT ( 'NONE',  ( -68.61029696402175659, 89.27050837028272667, 68.20127528263711270 ) ) ;
#15987 = FACE_OUTER_BOUND ( 'NONE', #18795, .T. ) ;
#15988 = VERTEX_POINT ( 'NONE', #20500 ) ;
#15989 = EDGE_CURVE ( 'NONE', #15089, #959, #6834, .T. ) ;
#15990 = CARTESIAN_POINT ( 'NONE',  ( -48.70980520421279181, 94.99786382055523859, -43.46127891409652477 ) ) ;
#15991 = ORIENTED_EDGE ( 'NONE', *, *, #18787, .F. ) ;
#15992 = CARTESIAN_POINT ( 'NONE',  ( 79.99331838321640475, 84.99999999999997158, -1.033931352371301848 ) ) ;
#15993 = CIRCLE ( 'NONE', #19979, 2.000000000000001332 ) ;
#15994 = DIRECTION ( 'NONE',  ( -5.440186201345738641E-18, -1.000000000000000000, -1.334940939666364181E-17 ) ) ;
#15995 = DIRECTION ( 'NONE',  ( 0.01292394549866738782, 0.005513023399720701559, 0.9999012842304693116 ) ) ;
#15996 = ADVANCED_FACE ( 'NONE', ( #13855 ), #16945, .F. ) ;
#15997 = VERTEX_POINT ( 'NONE', #4879 ) ;
#15998 = CARTESIAN_POINT ( 'NONE',  ( 13.80637996605699769, 137.5572120012638777, 100.9913744321402902 ) ) ;
#15999 = LINE ( 'NONE', #21671, #11578 ) ;
#16000 = CARTESIAN_POINT ( 'NONE',  ( 21.12819794574845389, 168.6979899673408738, 317.6497408708420380 ) ) ;
#16001 = ADVANCED_FACE ( 'NONE', ( #15486 ), #11919, .F. ) ;
#16002 = ORIENTED_EDGE ( 'NONE', *, *, #7116, .T. ) ;
#16003 = ADVANCED_FACE ( 'NONE', ( #6728 ), #17305, .T. ) ;
#16004 = DIRECTION ( 'NONE',  ( 0.4654428868037414624, 0.8850574712643624053, -0.006015952371159205558 ) ) ;
#16005 = EDGE_CURVE ( 'NONE', #5517, #16093, #16289, .T. ) ;
#16006 = CARTESIAN_POINT ( 'NONE',  ( -88.16630077365425677, 88.52135011679131082, 52.66304911287246426 ) ) ;
#16007 = EDGE_CURVE ( 'NONE', #19370, #8189, #16215, .T. ) ;
#16008 = VECTOR ( 'NONE', #18694, 1000.000000000000000 ) ;
#16010 = ORIENTED_EDGE ( 'NONE', *, *, #15278, .T. ) ;
#16009 = ORIENTED_EDGE ( 'NONE', *, *, #14709, .F. ) ;
#16011 = ORIENTED_EDGE ( 'NONE', *, *, #1278, .T. ) ;
#16012 = DIRECTION ( 'NONE',  ( -0.4397038457472313144, 0.000000000000000000, -0.8981428216242086648 ) ) ;
#16013 = FACE_OUTER_BOUND ( 'NONE', #3445, .T. ) ;
#16014 = CARTESIAN_POINT ( 'NONE',  ( -53.01407513488474876, 118.5884715842524457, 107.5779438241560655 ) ) ;
#16015 = ADVANCED_FACE ( 'NONE', ( #526 ), #10675, .T. ) ;
#16016 = CARTESIAN_POINT ( 'NONE',  ( -58.84901841222320229, 118.8937358571614453, 163.0286266904498405 ) ) ;
#16017 = ORIENTED_EDGE ( 'NONE', *, *, #4753, .T. ) ;
#16018 = ADVANCED_FACE ( 'NONE', ( #14448 ), #17655, .F. ) ;
#16019 = DIRECTION ( 'NONE',  ( -0.01292394549866632963, -0.005513023399716958026, -0.9999012842304692006 ) ) ;
#16020 = ORIENTED_EDGE ( 'NONE', *, *, #11970, .F. ) ;
#16021 = CARTESIAN_POINT ( 'NONE',  ( -56.62045793664813687, 114.4475724922177733, 172.8470550438757414 ) ) ;
#16022 = CARTESIAN_POINT ( 'NONE',  ( -48.91844876508264406, 94.45452722259994971, 84.00069590936301722 ) ) ;
#16023 = DIRECTION ( 'NONE',  ( -0.02100262710018139731, 0.02843993988601858577, -0.9993748343210220320 ) ) ;
#16024 = CARTESIAN_POINT ( 'NONE',  ( -25.88280235575286170, 324.3728210164380243, 319.3441878704100532 ) ) ;
#16025 = ORIENTED_EDGE ( 'NONE', *, *, #406, .T. ) ;
#16026 = FACE_OUTER_BOUND ( 'NONE', #15042, .T. ) ;
#16027 = DIRECTION ( 'NONE',  ( 0.9999164797902017066, 6.965998958219365988E-18, -0.01292414190464157356 ) ) ;
#16028 = CARTESIAN_POINT ( 'NONE',  ( -14.37471740060550118, 109.6998846769365628, 127.3137863664913425 ) ) ;
#16029 = VECTOR ( 'NONE', #3439, 1000.000000000000227 ) ;
#16030 = LINE ( 'NONE', #19094, #15458 ) ;
#16031 = ORIENTED_EDGE ( 'NONE', *, *, #18770, .F. ) ;
#16032 = DIRECTION ( 'NONE',  ( -0.8981428216242028917, -0.000000000000000000, -0.4397038457472429718 ) ) ;
#16033 = ORIENTED_EDGE ( 'NONE', *, *, #12181, .T. ) ;
#16034 = EDGE_LOOP ( 'NONE', ( #4123, #13188, #10729, #7480 ) ) ;
#16035 = APPLICATION_CONTEXT ( 'automotive_design' ) ;
#16036 = DIRECTION ( 'NONE',  ( -7.125109674161259066E-05, 0.9999848031710252272, -0.005512562950850163727 ) ) ;
#16037 = EDGE_CURVE ( 'NONE', #99, #12157, #2616, .T. ) ;
#16038 = ORIENTED_EDGE ( 'NONE', *, *, #21695, .T. ) ;
#16039 = DIRECTION ( 'NONE',  ( 1.000000000000000000, -0.000000000000000000, -9.912705577010318154E-17 ) ) ;
#16040 = LINE ( 'NONE', #21278, #5921 ) ;
#16041 = CARTESIAN_POINT ( 'NONE',  ( -91.34835587841297411, 70.11688414259907631, 61.28278498586107759 ) ) ;
#16042 = CARTESIAN_POINT ( 'NONE',  ( -38.21549050681395698, 167.4026153394593734, 273.1339171915171846 ) ) ;
#16043 = LINE ( 'NONE', #14433, #17942 ) ;
#16044 = CARTESIAN_POINT ( 'NONE',  ( -40.39453254641149726, 94.54797109823962842, 83.85657225284745664 ) ) ;
#16045 = EDGE_CURVE ( 'NONE', #18202, #16236, #17993, .T. ) ;
#16046 = PRODUCT ( 'Square Thread Nut', 'Square Thread Nut', '', ( #12664 ) ) ;
#16047 = CARTESIAN_POINT ( 'NONE',  ( -88.18706637290659955, 88.71869973106718987, 50.32066939225188662 ) ) ;
#16048 = CARTESIAN_POINT ( 'NONE',  ( 18.83139044548908814, 185.0137141601130111, 311.0664150449422891 ) ) ;
#16049 = CARTESIAN_POINT ( 'NONE',  ( 92.11236706770203853, 79.08401524093144985, 26.36688770261577375 ) ) ;
#16050 = CARTESIAN_POINT ( 'NONE',  ( -83.95054225259529801, 104.7585062753441463, -71.08029813247938478 ) ) ;
#16051 = VERTEX_POINT ( 'NONE', #17536 ) ;
#16052 = CARTESIAN_POINT ( 'NONE',  ( -9.634491729107175217, 187.4432466547973490, 321.1725384739820015 ) ) ;
#16053 = DIRECTION ( 'NONE',  ( -0.9934404589540163366, -0.1135548637187053511, 0.01346653032743023309 ) ) ;
#16054 = ORIENTED_EDGE ( 'NONE', *, *, #9184, .F. ) ;
#16055 = DIRECTION ( 'NONE',  ( -0.9999164797902015955, 0.000000000000000000, 0.01292414190464162733 ) ) ;
#16056 = VERTEX_POINT ( 'NONE', #12476 ) ;
#16057 = VERTEX_POINT ( 'NONE', #19676 ) ;
#16058 = ADVANCED_FACE ( 'NONE', ( #7065 ), #6291, .T. ) ;
#16059 = EDGE_CURVE ( 'NONE', #20863, #11327, #414, .T. ) ;
#16060 = ORIENTED_EDGE ( 'NONE', *, *, #14165, .T. ) ;
#16061 = CARTESIAN_POINT ( 'NONE',  ( 41.58451242677340076, 92.58578643762696458, 83.88377541325534992 ) ) ;
#16062 = DIRECTION ( 'NONE',  ( -0.000000000000000000, -1.000000000000000000, -0.000000000000000000 ) ) ;
#16063 = FACE_OUTER_BOUND ( 'NONE', #21798, .T. ) ;
#16064 = DIRECTION ( 'NONE',  ( -7.125109674025824596E-05, 0.9999848031710253382, -0.005512562950849464634 ) ) ;
#16065 = ORIENTED_EDGE ( 'NONE', *, *, #2892, .T. ) ;
#16066 = DIRECTION ( 'NONE',  ( 0.3101392564284309317, 0.9506461370142480494, -0.009250070373105347826 ) ) ;
#16067 = ORIENTED_EDGE ( 'NONE', *, *, #4620, .F. ) ;
#16068 = ORIENTED_EDGE ( 'NONE', *, *, #2239, .F. ) ;
#16069 = CARTESIAN_POINT ( 'NONE',  ( 26.56914632585049674, 169.3906321239456361, -110.8833952302934023 ) ) ;
#16070 = CARTESIAN_POINT ( 'NONE',  ( -61.06315242452672010, 118.9229714579762742, 168.3606140555295951 ) ) ;
#16071 = PRODUCT_RELATED_PRODUCT_CATEGORY ( 'part', '', ( #21141 ) ) ;
#16072 = CIRCLE ( 'NONE', #21877, 4.999999999999990230 ) ;
#16073 = LINE ( 'NONE', #21315, #7317 ) ;
#16074 = CARTESIAN_POINT ( 'NONE',  ( -14.82979117956944037, 177.4987173824078468, 90.64024647396865930 ) ) ;
#16075 = LINE ( 'NONE', #5586, #5600 ) ;
#16076 = CARTESIAN_POINT ( 'NONE',  ( 90.40889375659912730, 72.00000000000000000, -33.17122784026042837 ) ) ;
#16077 = ORIENTED_EDGE ( 'NONE', *, *, #3017, .T. ) ;
#16078 = CARTESIAN_POINT ( 'NONE',  ( -15.10364691323318453, 179.7443129775531077, 313.4557914687290463 ) ) ;
#16079 = ORIENTED_EDGE ( 'NONE', *, *, #666, .F. ) ;
#16080 = CARTESIAN_POINT ( 'NONE',  ( -90.40889375659909888, 78.43035437438882695, 33.17122784026039994 ) ) ;
#16081 = CARTESIAN_POINT ( 'NONE',  ( -3.321556572323998591, 326.9070248174119797, 307.9735416348814852 ) ) ;
#16082 = CARTESIAN_POINT ( 'NONE',  ( -15.06363346259513314, 179.7749131191535525, 316.0688698145405056 ) ) ;
#16083 = FACE_OUTER_BOUND ( 'NONE', #12917, .T. ) ;
#16084 = ORIENTED_EDGE ( 'NONE', *, *, #13617, .F. ) ;
#16085 = CIRCLE ( 'NONE', #14241, 2.499999999999988010 ) ;
#16086 = DIRECTION ( 'NONE',  ( 7.125109674364534776E-05, -0.9999848031710252272, 0.005512562950849704893 ) ) ;
#16087 = CONTEXT_DEPENDENT_SHAPE_REPRESENTATION ( #15893, #18908 ) ;
#16088 = VERTEX_POINT ( 'NONE', #12595 ) ;
#16089 = FACE_OUTER_BOUND ( 'NONE', #14976, .T. ) ;
#16090 = CARTESIAN_POINT ( 'NONE',  ( 93.21002351426729149, 69.99999999999998579, 28.79774562292276840 ) ) ;
#16091 = FACE_OUTER_BOUND ( 'NONE', #3308, .T. ) ;
#16092 = AXIS2_PLACEMENT_3D ( 'NONE', #4653, #22442, #8660 ) ;
#16093 = VERTEX_POINT ( 'NONE', #5215 ) ;
#16094 = CARTESIAN_POINT ( 'NONE',  ( 88.47461587451594767, 99.92585618460377361, -65.36342861369395507 ) ) ;
#16095 = CARTESIAN_POINT ( 'NONE',  ( 1.717753310876221295, 45.00000000000000000, 109.6869605904137330 ) ) ;
#16096 = ADVANCED_FACE ( 'NONE', ( #16167 ), #410, .T. ) ;
#16097 = ORIENTED_EDGE ( 'NONE', *, *, #17396, .T. ) ;
#16098 = CARTESIAN_POINT ( 'NONE',  ( 64.05646218218323895, 104.4142135623730780, -73.41979328131711213 ) ) ;
#16099 = ORIENTED_EDGE ( 'NONE', *, *, #3005, .T. ) ;
#16100 = DIRECTION ( 'NONE',  ( 0.9999164797902017066, 6.965998958219365988E-18, -0.01292414190464157356 ) ) ;
#16101 = LINE ( 'NONE', #14379, #11549 ) ;
#16102 = DIRECTION ( 'NONE',  ( -0.000000000000000000, -1.000000000000000000, -0.000000000000000000 ) ) ;
#16103 = PLANE ( 'NONE',  #3732 ) ;
#16104 =( GEOMETRIC_REPRESENTATION_CONTEXT ( 3 ) GLOBAL_UNCERTAINTY_ASSIGNED_CONTEXT ( ( #15922 ) ) GLOBAL_UNIT_ASSIGNED_CONTEXT ( ( #11322, #14798, #21854 ) ) REPRESENTATION_CONTEXT ( 'NONE', 'WORKASPACE' ) );
#16105 = CARTESIAN_POINT ( 'NONE',  ( 10.24508981178217937, 143.0941829715302731, 275.1657397502952449 ) ) ;
#16106 = CARTESIAN_POINT ( 'NONE',  ( -0.8458322068501320512, 327.1987054268951169, 310.0943410453546107 ) ) ;
#16107 = CARTESIAN_POINT ( 'NONE',  ( -51.99565694909051672, 170.0000000000000284, 0.6720553790413400508 ) ) ;
#16108 = EDGE_LOOP ( 'NONE', ( #10356, #8525, #17490, #542, #20098 ) ) ;
#16109 = CONICAL_SURFACE ( 'NONE', #22647, 9.000000000000001776, 1.047197551196594301 ) ;
#16110 = ADVANCED_FACE ( 'NONE', ( #12251 ), #8896, .T. ) ;
#16111 = CARTESIAN_POINT ( 'NONE',  ( -56.88982296092818558, 126.2575686056375304, 47.57983110662539161 ) ) ;
#16112 = CARTESIAN_POINT ( 'NONE',  ( -90.04909287368641913, 87.61728352428917788, 51.02202590385057590 ) ) ;
#16113 = EDGE_CURVE ( 'NONE', #16183, #6890, #5162, .T. ) ;
#16114 = VECTOR ( 'NONE', #14274, 1000.000000000000114 ) ;
#16115 = CIRCLE ( 'NONE', #7653, 5.100000000000000533 ) ;
#16116 = ORIENTED_EDGE ( 'NONE', *, *, #1925, .F. ) ;
#16117 = EDGE_LOOP ( 'NONE', ( #20435, #15720, #7610, #1436 ) ) ;
#16118 = SPHERICAL_SURFACE ( 'NONE', #14394, 11.00000000000000533 ) ;
#16119 = LINE ( 'NONE', #361, #1212 ) ;
#16120 = VERTEX_POINT ( 'NONE', #21409 ) ;
#16121 = DIRECTION ( 'NONE',  ( -0.9999164797902015955, -6.965998958219364448E-18, 0.01292414190464157182 ) ) ;
#16122 = CARTESIAN_POINT ( 'NONE',  ( -53.12394241931270500, 114.6366640169135849, 162.3035455873394426 ) ) ;
#16123 = EDGE_CURVE ( 'NONE', #160, #2284, #21651, .T. ) ;
#16124 = ORIENTED_EDGE ( 'NONE', *, *, #9811, .T. ) ;
#16125 = CARTESIAN_POINT ( 'NONE',  ( -3.593002051346241288, 173.4481159825171233, 324.6582153119202871 ) ) ;
#16126 = EDGE_LOOP ( 'NONE', ( #14187, #16394, #12408, #19935, #4966 ) ) ;
#16127 = DIRECTION ( 'NONE',  ( 0.3101392564284310982, 0.9506461370142479383, -0.009250070373107712254 ) ) ;
#16128 = EDGE_CURVE ( 'NONE', #9044, #19287, #10863, .T. ) ;
#16129 = CARTESIAN_POINT ( 'NONE',  ( 19.14152124230007956, 177.4876913356084174, 88.20102308074991981 ) ) ;
#16130 = CARTESIAN_POINT ( 'NONE',  ( -79.72222561103433236, 75.13699351169601925, -4.069998570383594583 ) ) ;
#16131 = CARTESIAN_POINT ( 'NONE',  ( -23.19743147896374680, 324.6326046529285350, 307.6196804043323709 ) ) ;
#16132 = AXIS2_PLACEMENT_3D ( 'NONE', #7584, #18383, #11374 ) ;
#16133 = CARTESIAN_POINT ( 'NONE',  ( -105.8709953322713631, 79.07548657612757381, 29.85559726770808808 ) ) ;
#16134 = ADVANCED_FACE ( 'NONE', ( #9237 ), #14212, .T. ) ;
#16135 = ORIENTED_EDGE ( 'NONE', *, *, #9891, .T. ) ;
#16136 = DIRECTION ( 'NONE',  ( 5.440186201345738641E-18, 1.000000000000000000, 1.334940939666364181E-17 ) ) ;
#16137 = DIRECTION ( 'NONE',  ( 7.125109674161246868E-05, -0.9999848031710252272, 0.005512562950850154186 ) ) ;
#16138 = VECTOR ( 'NONE', #20193, 1000.000000000000000 ) ;
#16139 = DIRECTION ( 'NONE',  ( -1.000000000000000000, -0.000000000000000000, 1.458023040593674599E-16 ) ) ;
#16140 = ORIENTED_EDGE ( 'NONE', *, *, #19495, .T. ) ;
#16141 = CARTESIAN_POINT ( 'NONE',  ( 162.0000000000000000, 0.000000000000000000, -2.262479907570351121E-12 ) ) ;
#16142 = ORIENTED_EDGE ( 'NONE', *, *, #17663, .T. ) ;
#16143 = VERTEX_POINT ( 'NONE', #5441 ) ;
#16144 = CARTESIAN_POINT ( 'NONE',  ( -85.09746116526416415, 74.99998524847651993, 0.7676313051536899357 ) ) ;
#16145 = DIRECTION ( 'NONE',  ( -0.01292394549866745720, -0.005513023399720816918, -0.9999012842304692006 ) ) ;
#16146 = ADVANCED_FACE ( 'NONE', ( #10750 ), #14736, .T. ) ;
#16147 = CLOSED_SHELL ( 'NONE', ( #22639, #4117, #17875, #20816, #16757, #437, #22398, #16858, #17217, #4270, #19474, #18491, #19776, #17542, #3723, #13160, #5716, #19609, #4012, #7098, #13461, #7306, #12974, #4973, #12444, #12483, #8466 ) ) ;
#16148 = AXIS2_PLACEMENT_3D ( 'NONE', #12146, #18915, #16999 ) ;
#16149 = EDGE_CURVE ( 'NONE', #11656, #11828, #17776, .T. ) ;
#16150 = EDGE_LOOP ( 'NONE', ( #4687, #3562, #3228, #17605 ) ) ;
#16151 = CARTESIAN_POINT ( 'NONE',  ( -36.90283430563165723, 95.89798883583559075, 85.13120909300619132 ) ) ;
#16152 = AXIS2_PLACEMENT_3D ( 'NONE', #8587, #15401, #5133 ) ;
#16153 = CARTESIAN_POINT ( 'NONE',  ( 1.466978256704031480, 165.6256992825491068, 113.4973404962053820 ) ) ;
#16154 = CARTESIAN_POINT ( 'NONE',  ( -13.16231198119108114, 149.0364497547966209, 278.8421488773936403 ) ) ;
#16155 = FACE_OUTER_BOUND ( 'NONE', #15077, .T. ) ;
#16156 = CARTESIAN_POINT ( 'NONE',  ( -38.81110560441968715, 96.91202807169366906, 84.24656211158296060 ) ) ;
#16157 = CARTESIAN_POINT ( 'NONE',  ( -64.19352405470968392, 87.93458184773491837, 62.81557474972223787 ) ) ;
#16158 = CARTESIAN_POINT ( 'NONE',  ( -64.99457118636313169, 170.0000000000000284, 0.8400692238016805868 ) ) ;
#16159 = CARTESIAN_POINT ( 'NONE',  ( 19.35430270680923925, 183.2211243877775075, 311.5661513781196845 ) ) ;
#16160 = CARTESIAN_POINT ( 'NONE',  ( 91.96840972750152332, 79.95771593962619761, 29.13399816620329830 ) ) ;
#16161 = CARTESIAN_POINT ( 'NONE',  ( 1.466978256704031480, 165.6256992825491068, 113.4973404962053820 ) ) ;
#16162 = EDGE_CURVE ( 'NONE', #9612, #11275, #20126, .T. ) ;
#16163 = ORIENTED_EDGE ( 'NONE', *, *, #10786, .T. ) ;
#16164 = AXIS2_PLACEMENT_3D ( 'NONE', #16699, #13238, #16905 ) ;
#16165 = CIRCLE ( 'NONE', #17241, 10.00000000000005684 ) ;
#16166 = DIRECTION ( 'NONE',  ( 0.009138748381789112835, -0.7071067811865462405, 0.7070477234798342447 ) ) ;
#16167 = FACE_OUTER_BOUND ( 'NONE', #9644, .T. ) ;
#16168 = AXIS2_PLACEMENT_3D ( 'NONE', #12977, #5596, #4211 ) ;
#16169 = EDGE_LOOP ( 'NONE', ( #16584, #17847, #834, #9959 ) ) ;
#16170 = FACE_OUTER_BOUND ( 'NONE', #20960, .T. ) ;
#16171 = ORIENTED_EDGE ( 'NONE', *, *, #22444, .T. ) ;
#16172 = EDGE_CURVE ( 'NONE', #3176, #6678, #854, .T. ) ;
#16173 = CIRCLE ( 'NONE', #20903, 110.0000000000000000 ) ;
#16174 = ORIENTED_EDGE ( 'NONE', *, *, #2638, .F. ) ;
#16175 = CARTESIAN_POINT ( 'NONE',  ( 14.14224087380716455, 105.6999953372425409, 126.9762993157022777 ) ) ;
#16176 = LINE ( 'NONE', #17894, #7999 ) ;
#16177 = PRODUCT_DEFINITION_CONTEXT ( 'detailed design', #14858, 'design' ) ;
#16178 = TOROIDAL_SURFACE ( 'NONE', #11765, 85.00000000000000000, 2.000000000000000000 ) ;
#16179 = DIRECTION ( 'NONE',  ( -0.01292394549866736873, -0.005513023399721228915, -0.9999012842304690896 ) ) ;
#16180 = DIRECTION ( 'NONE',  ( -0.9999164797902015955, -6.965998958219364448E-18, 0.01292414190464157182 ) ) ;
#16181 = VECTOR ( 'NONE', #20245, 1000.000000000000114 ) ;
#16182 = CARTESIAN_POINT ( 'NONE',  ( 11.80593078190077883, 176.3657686503914874, 324.4440941186779810 ) ) ;
#16183 = VERTEX_POINT ( 'NONE', #21737 ) ;
#16184 = CARTESIAN_POINT ( 'NONE',  ( 12.28794424968258170, 188.3253985970229678, 320.9523548641618049 ) ) ;
#16185 = VERTEX_POINT ( 'NONE', #11547 ) ;
#16186 = EDGE_LOOP ( 'NONE', ( #7903, #16581, #6655, #12596 ) ) ;
#16187 = CARTESIAN_POINT ( 'NONE',  ( -91.34851551837614636, 77.30892464375351381, 31.47853330177474618 ) ) ;
#16188 = DIRECTION ( 'NONE',  ( -0.01292394549866738261, -0.005513023399719314648, -0.9999012842304692006 ) ) ;
#16189 = CARTESIAN_POINT ( 'NONE',  ( 67.64952533873932339, 70.35418627987229456, -86.73849053056652281 ) ) ;
#16190 = EDGE_CURVE ( 'NONE', #19220, #8205, #4398, .T. ) ;
#16191 = CARTESIAN_POINT ( 'NONE',  ( -9.161099694250802727, 184.8065847297386881, 323.2196502909779952 ) ) ;
#16192 = AXIS2_PLACEMENT_3D ( 'NONE', #21408, #8765, #7180 ) ;
#16193 = EDGE_CURVE ( 'NONE', #11876, #20544, #2703, .T. ) ;
#16194 = CARTESIAN_POINT ( 'NONE',  ( -92.29888966083511548, 77.12912189587409273, 31.19548940143700833 ) ) ;
#16195 = CARTESIAN_POINT ( 'NONE',  ( 58.84248781247372762, 143.5743091050291298, 103.4941650606791512 ) ) ;
#16196 = ORIENTED_EDGE ( 'NONE', *, *, #7978, .F. ) ;
#16197 = CARTESIAN_POINT ( 'NONE',  ( -12.81093929260451780, 184.2871116315758115, 320.0335541037995313 ) ) ;
#16198 = FACE_OUTER_BOUND ( 'NONE', #19017, .T. ) ;
#16199 = CARTESIAN_POINT ( 'NONE',  ( -14.18925437717659577, 181.7892865527765025, 318.4638477695755796 ) ) ;
#16200 = ORIENTED_EDGE ( 'NONE', *, *, #7852, .F. ) ;
#16201 = CIRCLE ( 'NONE', #6989, 4.500000000000006217 ) ;
#16202 = VECTOR ( 'NONE', #3824, 999.9999999999998863 ) ;
#16203 =( REPRESENTATION_RELATIONSHIP ('NONE','NONE', #11808, #15770 ) REPRESENTATION_RELATIONSHIP_WITH_TRANSFORMATION ( #19827 )SHAPE_REPRESENTATION_RELATIONSHIP( ) );
#16204 = DIRECTION ( 'NONE',  ( -7.125109674161242803E-05, 0.9999848031710252272, -0.005512562950850150717 ) ) ;
#16205 = VECTOR ( 'NONE', #2052, 999.9999999999998863 ) ;
#16206 = ORIENTED_EDGE ( 'NONE', *, *, #21003, .T. ) ;
#16207 = CARTESIAN_POINT ( 'NONE',  ( 11.93555147538424777, 188.0368403985024486, 306.1756385059576360 ) ) ;
#16208 = VECTOR ( 'NONE', #15846, 999.9999999999998863 ) ;
#16209 = CONTEXT_DEPENDENT_SHAPE_REPRESENTATION ( #15016, #5145 ) ;
#16210 = DIRECTION ( 'NONE',  ( 0.9934404589540163366, 0.1135548637187051429, -0.01346653032743023309 ) ) ;
#16211 = CARTESIAN_POINT ( 'NONE',  ( -64.99457118636308905, 169.9999999999999716, 0.8400692238016759239 ) ) ;
#16212 = PLANE ( 'NONE',  #22081 ) ;
#16213 = ORIENTED_EDGE ( 'NONE', *, *, #4916, .F. ) ;
#16214 = CARTESIAN_POINT ( 'NONE',  ( 4.306364041547310784, 70.55846734465492887, -98.35747069930887676 ) ) ;
#16215 = CIRCLE ( 'NONE', #16923, 1.999999999999999778 ) ;
#16216 = ADVANCED_FACE ( 'NONE', ( #19785 ), #21845, .F. ) ;
#16217 = CARTESIAN_POINT ( 'NONE',  ( -50.54267232652800601, 95.91485852618909291, -44.96266421069820041 ) ) ;
#16218 = ORIENTED_EDGE ( 'NONE', *, *, #10520, .F. ) ;
#16219 = CARTESIAN_POINT ( 'NONE',  ( -47.94869851243297632, 168.6907664596094776, 35.22912207911639371 ) ) ;
#16220 = CIRCLE ( 'NONE', #2618, 2.000000000000001776 ) ;
#16221 = CARTESIAN_POINT ( 'NONE',  ( 51.99565694909048830, 170.0000000000000284, -0.6720553790413839046 ) ) ;
#16222 = VECTOR ( 'NONE', #4511, 1000.000000000000114 ) ;
#16223 = CARTESIAN_POINT ( 'NONE',  ( -42.42378443038275293, 94.99786382055523859, -43.54252712446056961 ) ) ;
#16224 = CARTESIAN_POINT ( 'NONE',  ( 3.898201936395599532, 166.6627968962365287, 301.5965304707955852 ) ) ;
#16225 = ORIENTED_EDGE ( 'NONE', *, *, #19012, .F. ) ;
#16226 = CARTESIAN_POINT ( 'NONE',  ( 0.000000000000000000, 20.00000000000000000, 0.000000000000000000 ) ) ;
#16227 = CIRCLE ( 'NONE', #20232, 2.000000000000001332 ) ;
#16228 = DIRECTION ( 'NONE',  ( -0.02033837109167978621, -0.03960957306447945164, -0.9990082243820552765 ) ) ;
#16229 = ORIENTED_EDGE ( 'NONE', *, *, #15393, .F. ) ;
#16230 = DIRECTION ( 'NONE',  ( 0.009760756503427210282, -0.9999378516499566327, 0.005387065077606872227 ) ) ;
#16231 = CIRCLE ( 'NONE', #16962, 101.0000000000000000 ) ;
#16232 = CARTESIAN_POINT ( 'NONE',  ( -88.18408833530436652, 88.91958178016859904, 50.72524270039643568 ) ) ;
#16233 = AXIS2_PLACEMENT_3D ( 'NONE', #2806, #9815, #16830 ) ;
#16234 =( LENGTH_UNIT ( ) NAMED_UNIT ( * ) SI_UNIT ( .MILLI., .METRE. ) );
#16235 = AXIS2_PLACEMENT_3D ( 'NONE', #20326, #3095, #4583 ) ;
#16236 = VERTEX_POINT ( 'NONE', #6138 ) ;
#16237 = VERTEX_POINT ( 'NONE', #6027 ) ;
#16238 = CARTESIAN_POINT ( 'NONE',  ( -5.563703806607757762, 326.7005119474488311, 320.3383740725303710 ) ) ;
#16239 = CARTESIAN_POINT ( 'NONE',  ( 41.56623493000981995, 91.17157287525387233, 82.46967996629568631 ) ) ;
#16240 = CARTESIAN_POINT ( 'NONE',  ( -106.2052848363077828, 71.73256685213067385, -28.64329287727204232 ) ) ;
#16241 = LINE ( 'NONE', #5861, #904 ) ;
#16242 = VERTEX_POINT ( 'NONE', #18551 ) ;
#16243 = DIRECTION ( 'NONE',  ( 0.9999164797902017066, 2.001050586450176344E-22, -0.01292414190464270286 ) ) ;
#16244 = VERTEX_POINT ( 'NONE', #6251 ) ;
#16245 = DIRECTION ( 'NONE',  ( 0.9999164797902017066, 2.001050586450178931E-22, -0.01292414190464131508 ) ) ;
#16246 = CARTESIAN_POINT ( 'NONE',  ( -91.23603883849614249, 78.43035437438885538, -30.82342686631250217 ) ) ;
#16247 = CARTESIAN_POINT ( 'NONE',  ( -78.60505072113932101, 75.12830914639056346, 5.952647260056409984 ) ) ;
#16248 = LINE ( 'NONE', #7597, #18762 ) ;
#16249 = AXIS2_PLACEMENT_3D ( 'NONE', #7121, #15995, #21015 ) ;
#16250 = ADVANCED_FACE ( 'NONE', ( #11088 ), #14666, .F. ) ;
#16251 = VECTOR ( 'NONE', #1130, 1000.000000000000000 ) ;
#16252 = FACE_OUTER_BOUND ( 'NONE', #16735, .T. ) ;
#16253 = CARTESIAN_POINT ( 'NONE',  ( 0.000000000000000000, 29.00000000000000355, 0.000000000000000000 ) ) ;
#16254 = DIRECTION ( 'NONE',  ( -0.01325671806966821978, 0.02938766274154132677, -0.9994801772444567023 ) ) ;
#16255 = CARTESIAN_POINT ( 'NONE',  ( 153.9999999999992610, 20.00000000000000000, -53.76161406891471017 ) ) ;
#16256 = EDGE_LOOP ( 'NONE', ( #14216, #19005, #6008, #1790 ) ) ;
#16257 = DIRECTION ( 'NONE',  ( -0.1296504907605108559, -0.005475273188901296634, -0.9915446392518419971 ) ) ;
#16258 = CIRCLE ( 'NONE', #12938, 4.000000000000002665 ) ;
#16259 = DIRECTION ( 'NONE',  ( -0.5121193912974635332, 0.6668151060996380108, -0.5413791123920870252 ) ) ;
#16260 = ORIENTED_EDGE ( 'NONE', *, *, #6526, .T. ) ;
#16261 = ORIENTED_EDGE ( 'NONE', *, *, #16037, .F. ) ;
#16262 = CARTESIAN_POINT ( 'NONE',  ( -84.00714561647235712, 75.05057272691709613, 4.197851120138568426 ) ) ;
#16263 = EDGE_CURVE ( 'NONE', #2761, #3975, #19468, .T. ) ;
#16264 = CARTESIAN_POINT ( 'NONE',  ( 92.46042328379809305, 77.12912189496645965, -29.19741020490909023 ) ) ;
#16265 = VECTOR ( 'NONE', #8749, 1000.000000000000000 ) ;
#16266 = ORIENTED_EDGE ( 'NONE', *, *, #7109, .T. ) ;
#16267 = VECTOR ( 'NONE', #20049, 1000.000000000000000 ) ;
#16268 = EDGE_CURVE ( 'NONE', #17449, #22622, #1161, .T. ) ;
#16269 = DIRECTION ( 'NONE',  ( 2.025474946048326158E-22, -1.000000000000000000, 1.876735158486679638E-22 ) ) ;
#16270 = CARTESIAN_POINT ( 'NONE',  ( -47.06729551376846388, 166.8517785085912237, 277.2517607094216032 ) ) ;
#16271 = CARTESIAN_POINT ( 'NONE',  ( -50.72033869335580647, 114.2302237440943742, 169.5554601261313223 ) ) ;
#16272 = DIRECTION ( 'NONE',  ( -5.440186201345738641E-18, -1.000000000000000000, -1.334940939666364181E-17 ) ) ;
#16273 = CARTESIAN_POINT ( 'NONE',  ( -39.54589198439538933, 93.83276874622022490, 84.56879583056640115 ) ) ;
#16274 = VECTOR ( 'NONE', #3312, 1000.000000000000000 ) ;
#16275 = DIRECTION ( 'NONE',  ( -0.3102455404053342525, -0.9506564598521393128, 0.000000000000000000 ) ) ;
#16276 = CARTESIAN_POINT ( 'NONE',  ( 45.19575868936945540, 125.3640259171584290, 246.9784031832207631 ) ) ;
#16277 = CLOSED_SHELL ( 'NONE', ( #8516, #4178, #14271, #18061, #6310, #14031, #18826, #1659, #9352, #7030, #19309, #10780 ) ) ;
#16278 = CARTESIAN_POINT ( 'NONE',  ( 18.14697571336121840, 185.8659025024385585, 310.2548099270366606 ) ) ;
#16279 = CARTESIAN_POINT ( 'NONE',  ( 89.59156723394411870, 79.74270461908912466, 28.48704982653681483 ) ) ;
#16280 = EDGE_CURVE ( 'NONE', #12054, #19674, #14551, .T. ) ;
#16281 = CARTESIAN_POINT ( 'NONE',  ( 11.66102052791742594, 176.1941894196976932, 323.4458143052556238 ) ) ;
#16282 = EDGE_CURVE ( 'NONE', #10034, #16304, #9354, .T. ) ;
#16283 = CARTESIAN_POINT ( 'NONE',  ( 1.421655609510571905, 105.0000000000000000, 109.9908127769221693 ) ) ;
#16284 = EDGE_CURVE ( 'NONE', #13612, #2375, #12521, .T. ) ;
#16285 = VECTOR ( 'NONE', #6298, 1000.000000000000114 ) ;
#16286 = EDGE_CURVE ( 'NONE', #719, #22322, #5906, .T. ) ;
#16287 = AXIS2_PLACEMENT_3D ( 'NONE', #5341, #302, #9014 ) ;
#16288 = DIRECTION ( 'NONE',  ( 0.01035335185279153900, 0.005513005182355262476, 0.9999312050732647172 ) ) ;
#16289 = LINE ( 'NONE', #9007, #3341 ) ;
#16290 = ORIENTED_EDGE ( 'NONE', *, *, #19221, .F. ) ;
#16291 = CARTESIAN_POINT ( 'NONE',  ( -89.70716773419725598, 79.66972452536272442, -28.26220109401206315 ) ) ;
#16292 = ORIENTED_EDGE ( 'NONE', *, *, #19931, .F. ) ;
#16293 = CARTESIAN_POINT ( 'NONE',  ( -1.208359178344593055, 144.6562660457661025, 274.7812028121480807 ) ) ;
#16294 = DIRECTION ( 'NONE',  ( 0.1337561903331546953, 0.9909881666746205298, -0.007192708699472573526 ) ) ;
#16295 = EDGE_CURVE ( 'NONE', #11132, #19478, #7373, .T. ) ;
#16296 = FACE_OUTER_BOUND ( 'NONE', #2290, .T. ) ;
#16297 = CARTESIAN_POINT ( 'NONE',  ( 52.34460878051607580, 84.99999999999997158, 26.32568957529409204 ) ) ;
#16298 = DIRECTION ( 'NONE',  ( -0.01292394549866737914, -0.005513023399721009472, -0.9999012842304692006 ) ) ;
#16299 = AXIS2_PLACEMENT_3D ( 'NONE', #16511, #18128, #13293 ) ;
#16300 = DIRECTION ( 'NONE',  ( 0.9232306267972776315, 0.000000000000000000, -0.3842462878721224495 ) ) ;
#16301 = CARTESIAN_POINT ( 'NONE',  ( 11.61857788991896179, 160.0893180226940444, 324.5352569096220918 ) ) ;
#16302 = DIRECTION ( 'NONE',  ( -0.01292394549866738608, -0.005513023399720699824, -0.9999012842304692006 ) ) ;
#16303 = DIRECTION ( 'NONE',  ( -0.01292394549866727679, -0.005513023399720743192, -0.9999012842304693116 ) ) ;
#16304 = VERTEX_POINT ( 'NONE', #11208 ) ;
#16305 = DIRECTION ( 'NONE',  ( 1.000000000000000000, 0.000000000000000000, 0.000000000000000000 ) ) ;
#16306 = CARTESIAN_POINT ( 'NONE',  ( 14.13996083871143306, 137.6995090387153482, 126.7998973012750810 ) ) ;
#16307 = CARTESIAN_POINT ( 'NONE',  ( 58.13288207869166513, 126.2713511641370445, 48.59330799816777358 ) ) ;
#16308 = EDGE_CURVE ( 'NONE', #5956, #15892, #10315, .T. ) ;
#16309 = CARTESIAN_POINT ( 'NONE',  ( 68.24431907518338392, 70.78648125535664803, -86.27145290589803039 ) ) ;
#16310 = CARTESIAN_POINT ( 'NONE',  ( 41.18784844526823719, 107.5071733437152375, 91.64309988731913847 ) ) ;
#16311 = LINE ( 'NONE', #2140, #8894 ) ;
#16312 = DIRECTION ( 'NONE',  ( -0.9232306267972774094, 0.000000000000000000, 0.3842462878721227826 ) ) ;
#16313 = AXIS2_PLACEMENT_3D ( 'NONE', #7883, #18233, #4538 ) ;
#16314 = EDGE_LOOP ( 'NONE', ( #14528, #16229, #17168, #19129 ) ) ;
#16315 = LINE ( 'NONE', #21535, #443 ) ;
#16316 = LINE ( 'NONE', #5591, #19792 ) ;
#16317 = CARTESIAN_POINT ( 'NONE',  ( -15.01362440653151786, 178.7143772909413713, 313.5209786370710958 ) ) ;
#16318 = ORIENTED_EDGE ( 'NONE', *, *, #6323, .F. ) ;
#16319 = ORIENTED_EDGE ( 'NONE', *, *, #16398, .T. ) ;
#16320 = VECTOR ( 'NONE', #4375, 1000.000000000000227 ) ;
#16321 = DIRECTION ( 'NONE',  ( 0.009760756503427813965, -0.9999378516499565217, 0.005387065077607405654 ) ) ;
#16322 = ORIENTED_EDGE ( 'NONE', *, *, #11932, .T. ) ;
#16323 = ORIENTED_EDGE ( 'NONE', *, *, #91, .T. ) ;
#16324 = DIRECTION ( 'NONE',  ( 0.000000000000000000, 0.000000000000000000, -1.000000000000000000 ) ) ;
#16325 = EDGE_CURVE ( 'NONE', #9627, #9437, #11888, .T. ) ;
#16326 = ITEM_DEFINED_TRANSFORMATION ( 'NONE', 'NONE', #19079,  #6292 ) ;
#16327 = CIRCLE ( 'NONE', #18494, 97.00000000000005684 ) ;
#16328 = DIRECTION ( 'NONE',  ( 7.125109674364536131E-05, -0.9999848031710253382, 0.005512562950849705760 ) ) ;
#16329 = CARTESIAN_POINT ( 'NONE',  ( -6.702556532201369599, 81.97459999999998104, -87.68700545388550438 ) ) ;
#16330 = VECTOR ( 'NONE', #7545, 999.9999999999998863 ) ;
#16331 = VERTEX_POINT ( 'NONE', #1435 ) ;
#16332 = AXIS2_PLACEMENT_3D ( 'NONE', #3143, #1438, #20938 ) ;
#16333 = FACE_OUTER_BOUND ( 'NONE', #13076, .T. ) ;
#16334 = ORIENTED_EDGE ( 'NONE', *, *, #13060, .T. ) ;
#16335 = LINE ( 'NONE', #14253, #6228 ) ;
#16336 = ORIENTED_EDGE ( 'NONE', *, *, #15162, .F. ) ;
#16337 = EDGE_LOOP ( 'NONE', ( #9539, #14371, #257, #18042 ) ) ;
#16338 = PLANE ( 'NONE',  #4464 ) ;
#16339 = DIRECTION ( 'NONE',  ( -0.01292394549866736179, -0.005513023399721110954, -0.9999012842304692006 ) ) ;
#16340 = CARTESIAN_POINT ( 'NONE',  ( -40.78795384167224825, 95.60340320854591312, -42.51611673894687016 ) ) ;
#16341 = CARTESIAN_POINT ( 'NONE',  ( -49.61360656010212722, 118.9155345184949653, 166.8635573802473857 ) ) ;
#16342 =( REPRESENTATION_RELATIONSHIP ('NONE','NONE', #11808, #15770 ) REPRESENTATION_RELATIONSHIP_WITH_TRANSFORMATION ( #22466 )SHAPE_REPRESENTATION_RELATIONSHIP( ) );
#16343 = DIRECTION ( 'NONE',  ( -0.9999164797902015955, -6.965998958219364448E-18, 0.01292414190464157182 ) ) ;
#16344 = AXIS2_PLACEMENT_3D ( 'NONE', #20405, #11592, #20303 ) ;
#16345 = CARTESIAN_POINT ( 'NONE',  ( 45.22132157597982882, 129.3749911766419700, 248.9561554998783208 ) ) ;
#16346 = VERTEX_POINT ( 'NONE', #8411 ) ;
#16347 = AXIS2_PLACEMENT_3D ( 'NONE', #17117, #11603, #9990 ) ;
#16348 = CARTESIAN_POINT ( 'NONE',  ( 42.78098668172552976, 106.8060942374655156, 70.38625157530108822 ) ) ;
#16349 = FACE_OUTER_BOUND ( 'NONE', #18478, .T. ) ;
#16350 = EDGE_CURVE ( 'NONE', #650, #16857, #11436, .T. ) ;
#16351 = APPLICATION_PROTOCOL_DEFINITION ( 'draft international standard', 'automotive_design', 1998, #19944 ) ;
#16352 = EDGE_CURVE ( 'NONE', #17835, #13946, #7657, .T. ) ;
#16353 = ORIENTED_EDGE ( 'NONE', *, *, #19556, .F. ) ;
#16354 = CYLINDRICAL_SURFACE ( 'NONE', #16132, 83.99999999999998579 ) ;
#16355 = CARTESIAN_POINT ( 'NONE',  ( -3.200698602031736950, 81.99999999999998579, -81.18156990192605349 ) ) ;
#16356 = ORIENTED_EDGE ( 'NONE', *, *, #10021, .F. ) ;
#16357 = CARTESIAN_POINT ( 'NONE',  ( -16.52952334881082663, 137.6261247937603969, 113.8843268131127218 ) ) ;
#16358 = DIRECTION ( 'NONE',  ( 0.6915547089979297013, -0.09853460026858011644, -0.7155718112200200043 ) ) ;
#16359 = CARTESIAN_POINT ( 'NONE',  ( 3.316624388958365088, 166.4147108432491109, 256.6009726804241495 ) ) ;
#16360 = CARTESIAN_POINT ( 'NONE',  ( 20.98757502854828516, 180.4221386788647123, 76.27757023658386970 ) ) ;
#16361 = DIRECTION ( 'NONE',  ( -7.125109674025824596E-05, 0.9999848031710253382, -0.005512562950849464634 ) ) ;
#16362 = EDGE_LOOP ( 'NONE', ( #12354, #7505, #12975, #79 ) ) ;
#16363 = DIRECTION ( 'NONE',  ( -0.01292394549866731843, -0.005513023399720594006, -0.9999012842304693116 ) ) ;
#16364 = ORIENTED_EDGE ( 'NONE', *, *, #16556, .T. ) ;
#16365 = DIRECTION ( 'NONE',  ( -0.01292414190464137060, 0.000000000000000000, -0.9999164797902015955 ) ) ;
#16366 = CARTESIAN_POINT ( 'NONE',  ( 50.04172213657920310, 189.5996388551388918, -73.32787460386838063 ) ) ;
#16367 = CARTESIAN_POINT ( 'NONE',  ( 48.35171741268020185, 162.6510295535512682, 256.0396354428399945 ) ) ;
#16368 = DIRECTION ( 'NONE',  ( 0.009760756503427210282, -0.9999378516499566327, 0.005387065077606872227 ) ) ;
#16369 = DIRECTION ( 'NONE',  ( -0.01292394549866741384, -0.005513023399720269613, -0.9999012842304692006 ) ) ;
#16370 = CARTESIAN_POINT ( 'NONE',  ( -11.23675596313486125, 155.5381941787832716, 97.81558748025743455 ) ) ;
#16371 = CARTESIAN_POINT ( 'NONE',  ( 53.22133760583491124, 119.7725967263615985, 248.9056969729654440 ) ) ;
#16372 = CARTESIAN_POINT ( 'NONE',  ( 39.89762790624313737, 105.6320600527179607, 91.75806838212221805 ) ) ;
#16373 = DIRECTION ( 'NONE',  ( -0.01292394549866750231, -0.005513023399722823126, -0.9999012842304692006 ) ) ;
#16374 = ORIENTED_EDGE ( 'NONE', *, *, #13140, .T. ) ;
#16375 = AXIS2_PLACEMENT_3D ( 'NONE', #9523, #17007, #6311 ) ;
#16376 = ORIENTED_EDGE ( 'NONE', *, *, #2625, .F. ) ;
#16377 = CARTESIAN_POINT ( 'NONE',  ( -81.70580161692535626, 75.12313863457445962, -3.781430161579881322 ) ) ;
#16378 = CARTESIAN_POINT ( 'NONE',  ( -90.15140406382808180, 88.04290212818831662, 53.09271965600965615 ) ) ;
#16379 = EDGE_CURVE ( 'NONE', #11822, #15528, #797, .T. ) ;
#16380 = ORIENTED_EDGE ( 'NONE', *, *, #14566, .F. ) ;
#16381 = CARTESIAN_POINT ( 'NONE',  ( -13.16231198119108114, 149.0364497547966209, 278.8421488773936403 ) ) ;
#16382 = CARTESIAN_POINT ( 'NONE',  ( -90.51972003054838467, 79.34791451281842001, -27.24428967784130862 ) ) ;
#16383 = ORIENTED_EDGE ( 'NONE', *, *, #17994, .F. ) ;
#16384 = DIRECTION ( 'NONE',  ( -0.9506032891036972909, 0.3102281881984321754, 0.01057629388542893900 ) ) ;
#16385 = CONICAL_SURFACE ( 'NONE', #12701, 11.00000000000000178, 0.7853981633974346233 ) ;
#16386 = CARTESIAN_POINT ( 'NONE',  ( 74.03668283561377450, 75.02057536297186857, -2.970158874850576947 ) ) ;
#16387 = CARTESIAN_POINT ( 'NONE',  ( 19.76541804458917539, 182.9254338870941297, 318.4526189355386236 ) ) ;
#16388 = CARTESIAN_POINT ( 'NONE',  ( 2.139116399059427742, 86.14745084375786632, -75.03391309205547088 ) ) ;
#16389 = EDGE_CURVE ( 'NONE', #2091, #19509, #5549, .T. ) ;
#16390 = CARTESIAN_POINT ( 'NONE',  ( -14.91027303991310404, 185.1232018939139436, 278.7355807953422300 ) ) ;
#16391 = EDGE_CURVE ( 'NONE', #20552, #10899, #20224, .T. ) ;
#16392 = CARTESIAN_POINT ( 'NONE',  ( 3.316624388958365088, 166.4147108432491109, 256.6009726804241495 ) ) ;
#16393 = DIRECTION ( 'NONE',  ( -0.9999164797902015955, -6.965998958219364448E-18, 0.01292414190464157182 ) ) ;
#16394 = ORIENTED_EDGE ( 'NONE', *, *, #17151, .T. ) ;
#16395 = VERTEX_POINT ( 'NONE', #4851 ) ;
#16396 = CARTESIAN_POINT ( 'NONE',  ( 49.22751544813647939, 112.6450176187863832, -44.82443924574226202 ) ) ;
#16397 = FACE_OUTER_BOUND ( 'NONE', #5669, .T. ) ;
#16398 = EDGE_CURVE ( 'NONE', #15431, #13179, #21085, .T. ) ;
#16399 = LINE ( 'NONE', #7414, #402 ) ;
#16400 = EDGE_CURVE ( 'NONE', #10705, #20064, #5183, .T. ) ;
#16401 = CARTESIAN_POINT ( 'NONE',  ( 75.60168123463965628, 75.03402262061140959, 1.580398487289465415 ) ) ;
#16402 = CYLINDRICAL_SURFACE ( 'NONE', #8876, 112.5000000000000142 ) ;
#16403 = DIRECTION ( 'NONE',  ( 0.01292414190463832269, 0.000000000000000000, 0.9999164797902017066 ) ) ;
#16404 = DIRECTION ( 'NONE',  ( 0.9999164797902015955, 6.965998958219364448E-18, -0.01292414190464157182 ) ) ;
#16405 = DIRECTION ( 'NONE',  ( 0.009760756503428008254, -0.9999378516499564107, 0.005387065077611006073 ) ) ;
#16406 = VERTEX_POINT ( 'NONE', #5075 ) ;
#16407 = DIRECTION ( 'NONE',  ( -0.9934404589540162256, -0.1135548637187057258, 0.01346653032743021748 ) ) ;
#16408 = CARTESIAN_POINT ( 'NONE',  ( 0.000000000000000000, 0.000000000000000000, 0.000000000000000000 ) ) ;
#16409 = CARTESIAN_POINT ( 'NONE',  ( 0.000000000000000000, 45.00000000000000000, 0.000000000000000000 ) ) ;
#16410 = EDGE_CURVE ( 'NONE', #3703, #4735, #11655, .T. ) ;
#16411 = CARTESIAN_POINT ( 'NONE',  ( 88.82392706003706451, 79.74373590868249551, -30.79623470077041247 ) ) ;
#16412 = FACE_OUTER_BOUND ( 'NONE', #12647, .T. ) ;
#16413 = CARTESIAN_POINT ( 'NONE',  ( -90.41053243085599433, 78.34173690304781701, 33.04444670410828877 ) ) ;
#16414 = SPHERICAL_SURFACE ( 'NONE', #4792, 2.000000000000000000 ) ;
#16415 = EDGE_LOOP ( 'NONE', ( #12957, #13464 ) ) ;
#16416 = CARTESIAN_POINT ( 'NONE',  ( -11.14887313374392264, 155.5756827379013885, 104.6149162130246282 ) ) ;
#16417 = B_SPLINE_CURVE_WITH_KNOTS ( 'NONE', 3,
 ( #21983, #21867, #7775, #4309, #1121, #18463, #4543, #5932, #21760, #18239, #11570, #20051, #1004, #16650, #18570, #19936 ),
 .UNSPECIFIED., .F., .F.,
 ( 4, 2, 2, 2, 2, 2, 2, 4 ),
 ( 0.000000000000000000, 0.0003951513861477968419, 0.0007903027722955936838, 0.001185454158443390634, 0.001580605544591187368, 0.001975756930738984101, 0.002370908316886781268, 0.003161211089182393817 ),
 .UNSPECIFIED. ) ;
#16418 = EDGE_CURVE ( 'NONE', #13170, #20174, #20817, .T. ) ;
#16419 = EDGE_LOOP ( 'NONE', ( #3749, #16673, #4677, #13522 ) ) ;
#16420 = DIRECTION ( 'NONE',  ( -0.9999164797902017066, 0.000000000000000000, 0.01292414190463832269 ) ) ;
#16421 = CARTESIAN_POINT ( 'NONE',  ( -13.17740673624774317, 181.2762379934293335, 309.7265655061761436 ) ) ;
#16422 = CIRCLE ( 'NONE', #4277, 112.5000000000007105 ) ;
#16423 = VERTEX_POINT ( 'NONE', #13499 ) ;
#16424 = ORIENTED_EDGE ( 'NONE', *, *, #15548, .T. ) ;
#16425 = DIRECTION ( 'NONE',  ( -0.1136178953597577479, 0.9935164314186355483, -0.004009283626633511344 ) ) ;
#16426 = LINE ( 'NONE', #789, #14038 ) ;
#16427 = EDGE_CURVE ( 'NONE', #18838, #19445, #8211, .T. ) ;
#16428 = ITEM_DEFINED_TRANSFORMATION ( 'NONE', 'NONE', #12869,  #6292 ) ;
#16429 = VECTOR ( 'NONE', #19954, 1000.000000000000227 ) ;
#16430 = LINE ( 'NONE', #12982, #3768 ) ;
#16431 = DIRECTION ( 'NONE',  ( 0.01292414190464131335, 1.902755938799530239E-22, 0.9999164797902015955 ) ) ;
#16432 = ORIENTED_EDGE ( 'NONE', *, *, #2080, .F. ) ;
#16433 = CARTESIAN_POINT ( 'NONE',  ( 81.88633517683543062, 104.6158228377113204, -73.44862222250269213 ) ) ;
#16434 = CARTESIAN_POINT ( 'NONE',  ( -14.62480137330870456, 179.3298053622281714, 309.9632843756066904 ) ) ;
#16435 = VERTEX_POINT ( 'NONE', #1328 ) ;
#16436 = CARTESIAN_POINT ( 'NONE',  ( -106.3114127004273257, 78.31407127224927933, -28.24702759725638401 ) ) ;
#16437 = DIRECTION ( 'NONE',  ( 0.000000000000000000, 1.000000000000000000, 0.000000000000000000 ) ) ;
#16438 = CARTESIAN_POINT ( 'NONE',  ( 2.830031787867825166, 81.99999999999998579, -80.39798906481894392 ) ) ;
#16439 = CARTESIAN_POINT ( 'NONE',  ( 20.71003051272330353, 88.26492295440642977, 77.04224443657528809 ) ) ;
#16440 = EDGE_LOOP ( 'NONE', ( #8403, #10025 ) ) ;
#16441 = ORIENTED_EDGE ( 'NONE', *, *, #8262, .F. ) ;
#16442 = EDGE_CURVE ( 'NONE', #1989, #2768, #15340, .T. ) ;
#16443 = CARTESIAN_POINT ( 'NONE',  ( 5.986268468634207807, 69.99999999999998579, -84.52572088931836447 ) ) ;
#16444 = CIRCLE ( 'NONE', #10550, 126.0000000000000000 ) ;
#16445 = DIRECTION ( 'NONE',  ( -0.8981428216242028917, 0.000000000000000000, 0.4397038457472432493 ) ) ;
#16446 = VERTEX_POINT ( 'NONE', #12108 ) ;
#16447 = UNCERTAINTY_MEASURE_WITH_UNIT (LENGTH_MEASURE( 1.000000000000000082E-05 ), #13592, 'distance_accuracy_value', 'NONE');
#16448 = DIRECTION ( 'NONE',  ( 7.125109674403276030E-05, -0.9999848031710252272, 0.005512562950848280685 ) ) ;
#16449 = CARTESIAN_POINT ( 'NONE',  ( -89.50624427484768830, 89.10716308766615157, 51.66467930733914926 ) ) ;
#16450 = ADVANCED_FACE ( 'NONE', ( #17753 ), #12566, .T. ) ;
#16451 = PRODUCT_CONTEXT ( 'NONE', #14106, 'mechanical' ) ;
#16453 = ORIENTED_EDGE ( 'NONE', *, *, #4813, .F. ) ;
#16452 = ORIENTED_EDGE ( 'NONE', *, *, #8673, .T. ) ;
#16454 = CYLINDRICAL_SURFACE ( 'NONE', #10605, 102.6746853779045381 ) ;
#16455 = CARTESIAN_POINT ( 'NONE',  ( -146.5000000000000000, 20.00000000000000000, 8.000000000000017764 ) ) ;
#16456 = ORIENTED_EDGE ( 'NONE', *, *, #11216, .F. ) ;
#16457 = FACE_OUTER_BOUND ( 'NONE', #12145, .T. ) ;
#16458 = CARTESIAN_POINT ( 'NONE',  ( 79.99331838321640475, 74.99899999999998101, -1.033931352371301404 ) ) ;
#16459 = CARTESIAN_POINT ( 'NONE',  ( -105.6473595942261028, 69.99999999999998579, -30.63715735456343126 ) ) ;
#16461 = CARTESIAN_POINT ( 'NONE',  ( 68.73688910937092089, 91.46348651515937433, -85.87923151210685546 ) ) ;
#16460 = APPLICATION_CONTEXT ( 'automotive_design' ) ;
#16462 = ORIENTED_EDGE ( 'NONE', *, *, #15423, .T. ) ;
#16463 = FACE_OUTER_BOUND ( 'NONE', #5186, .T. ) ;
#16464 = ORIENTED_EDGE ( 'NONE', *, *, #62, .F. ) ;
#16465 = DIRECTION ( 'NONE',  ( 0.01292414190464131508, 1.902755938799530474E-22, 0.9999164797902017066 ) ) ;
#16466 = CARTESIAN_POINT ( 'NONE',  ( -91.57598704441285520, 77.66227243743314546, -29.67486887243845572 ) ) ;
#16467 = CARTESIAN_POINT ( 'NONE',  ( 58.84248781247372762, 143.5743091050291298, 103.4941650606791370 ) ) ;
#16468 = CARTESIAN_POINT ( 'NONE',  ( -22.66159625276162970, 324.6936785073799001, 307.5691494985305781 ) ) ;
#16469 = CARTESIAN_POINT ( 'NONE',  ( 3.545303425248413465, 81.99999999999998579, -91.95213924926606808 ) ) ;
#16470 = EDGE_LOOP ( 'NONE', ( #357, #3509, #5302, #993 ) ) ;
#16471 = ADVANCED_FACE ( 'NONE', ( #12451, #8637 ), #1998, .F. ) ;
#16472 = DIRECTION ( 'NONE',  ( -0.4768814951561130555, 0.000000000000000000, -0.8789675987075236119 ) ) ;
#16473 = CARTESIAN_POINT ( 'NONE',  ( -7.475646132950418021, 81.19615242270661781, -81.73701953211944726 ) ) ;
#16474 = EDGE_CURVE ( 'NONE', #5966, #7339, #19487, .T. ) ;
#16475 = CARTESIAN_POINT ( 'NONE',  ( 39.48249285872903158, 105.5238643664723668, 91.68783210470924416 ) ) ;
#16476 = ORIENTED_EDGE ( 'NONE', *, *, #641, .F. ) ;
#16477 = DIRECTION ( 'NONE',  ( -7.125109674403837105E-05, 0.9999848031710252272, -0.005512562950847867821 ) ) ;
#16478 = DIRECTION ( 'NONE',  ( -0.9999164797902015955, -6.965998958219364448E-18, 0.01292414190464157182 ) ) ;
#16479 = ORIENTED_EDGE ( 'NONE', *, *, #13075, .T. ) ;
#16480 = VECTOR ( 'NONE', #21062, 1000.000000000000000 ) ;
#16481 = CARTESIAN_POINT ( 'NONE',  ( -90.11733922844207711, 88.39270497821426886, 52.83690678703658961 ) ) ;
#16482 = ORIENTED_EDGE ( 'NONE', *, *, #7665, .F. ) ;
#16483 = ORIENTED_EDGE ( 'NONE', *, *, #6427, .F. ) ;
#16484 = FACE_OUTER_BOUND ( 'NONE', #5922, .T. ) ;
#16485 = DIRECTION ( 'NONE',  ( -0.000000000000000000, -1.000000000000000000, -0.000000000000000000 ) ) ;
#16486 = VECTOR ( 'NONE', #11981, 1000.000000000000114 ) ;
#16487 = CYLINDRICAL_SURFACE ( 'NONE', #10044, 2.499999999999988010 ) ;
#16488 = CARTESIAN_POINT ( 'NONE',  ( 2.945655833907555810, 177.7182771800350167, 324.5501578882025910 ) ) ;
#16489 = AXIS2_PLACEMENT_3D ( 'NONE', #18625, #18527, #1409 ) ;
#16490 = CARTESIAN_POINT ( 'NONE',  ( 0.000000000000000000, 20.00000000000000000, 0.000000000000000000 ) ) ;
#16491 = DIRECTION ( 'NONE',  ( 0.4397038457472313144, 0.000000000000000000, 0.8981428216242086648 ) ) ;
#16492 = CARTESIAN_POINT ( 'NONE',  ( 19.91678837892234810, 183.5273396323361794, 313.8466901984123751 ) ) ;
#16493 = CARTESIAN_POINT ( 'NONE',  ( 92.91045972105432327, 79.04398536109876261, 26.22408268756185734 ) ) ;
#16494 = CARTESIAN_POINT ( 'NONE',  ( -41.63647828013468910, 161.7789141790872804, 257.2075612646602281 ) ) ;
#16495 = ORIENTED_EDGE ( 'NONE', *, *, #569, .F. ) ;
#16496 = DIRECTION ( 'NONE',  ( -2.025474946048326158E-22, 1.000000000000000000, -1.876735158486679638E-22 ) ) ;
#16497 = DIRECTION ( 'NONE',  ( -0.9999164797902017066, -2.001050586450177285E-22, 0.01292414190464218071 ) ) ;
#16498 = ORIENTED_EDGE ( 'NONE', *, *, #21689, .T. ) ;
#16499 = DIRECTION ( 'NONE',  ( -0.9934404589540163366, -0.1135548637187058507, 0.01346653032743036667 ) ) ;
#16500 = VERTEX_POINT ( 'NONE', #19657 ) ;
#16501 = TOROIDAL_SURFACE ( 'NONE', #13548, 93.00000000000000000, 2.000000000000000000 ) ;
#16502 = ORIENTED_EDGE ( 'NONE', *, *, #19417, .T. ) ;
#16503 = LINE ( 'NONE', #13068, #13392 ) ;
#16504 = CIRCLE ( 'NONE', #20861, 9.000000000000001776 ) ;
#16505 = ORIENTED_EDGE ( 'NONE', *, *, #1244, .F. ) ;
#16506 = DIRECTION ( 'NONE',  ( 0.7912924530843117310, -0.6113994113550570431, -0.006856638134102506846 ) ) ;
#16507 = CARTESIAN_POINT ( 'NONE',  ( 76.57033985922889485, 75.07731437015505094, -4.829186743783990821 ) ) ;
#16508 = SHAPE_REPRESENTATION ( 'Stud', ( #6292 ), #6306 ) ;
#16509 = DIRECTION ( 'NONE',  ( 0.9999164797902017066, 2.001050586450178931E-22, -0.01292414190464131508 ) ) ;
#16510 = DIRECTION ( 'NONE',  ( 0.01292394549866739996, 0.005513023399721131770, 0.9999012842304692006 ) ) ;
#16511 = CARTESIAN_POINT ( 'NONE',  ( -41.47069032946998846, 166.0668615304125808, 273.1833561390217824 ) ) ;
#16512 = EDGE_LOOP ( 'NONE', ( #15387, #10136, #2563, #7220 ) ) ;
#16513 = CARTESIAN_POINT ( 'NONE',  ( 1.364374644014609697E-14, 69.99999999999998579, -9.836443712999143722E-15 ) ) ;
#16514 = CARTESIAN_POINT ( 'NONE',  ( 0.000000000000000000, 0.000000000000000000, 0.000000000000000000 ) ) ;
#16515 = CARTESIAN_POINT ( 'NONE',  ( 89.38692540128420205, 98.12169273169054406, -64.10929978113784955 ) ) ;
#16516 = CARTESIAN_POINT ( 'NONE',  ( -53.72553639016752669, 114.2880042629071227, 172.4694075787558631 ) ) ;
#16517 = VECTOR ( 'NONE', #8225, 999.9999999999998863 ) ;
#16518 = ADVANCED_FACE ( 'NONE', ( #162, #3924, #5192 ), #3589, .T. ) ;
#16519 = VECTOR ( 'NONE', #3010, 1000.000000000000114 ) ;
#16520 = PLANE ( 'NONE',  #20164 ) ;
#16521 = LINE ( 'NONE', #19811, #19135 ) ;
#16522 = DIRECTION ( 'NONE',  ( -0.01292414190464023262, 0.000000000000000000, -0.9999164797902017066 ) ) ;
#16523 = CARTESIAN_POINT ( 'NONE',  ( -11.19281454843939194, 155.5569384583423300, 101.2152518466410243 ) ) ;
#16524 = ORIENTED_EDGE ( 'NONE', *, *, #3754, .T. ) ;
#16525 = EDGE_CURVE ( 'NONE', #10199, #7779, #7389, .T. ) ;
#16526 = DIRECTION ( 'NONE',  ( 0.9232306267972774094, 0.000000000000000000, -0.3842462878721227826 ) ) ;
#16527 = ADVANCED_FACE ( 'NONE', ( #5653 ), #11076, .F. ) ;
#16528 = ORIENTED_EDGE ( 'NONE', *, *, #5826, .F. ) ;
#16529 = LINE ( 'NONE', #1006, #1135 ) ;
#16530 = CARTESIAN_POINT ( 'NONE',  ( -10.03417356088257506, 184.3143220770519122, 308.0707497775335355 ) ) ;
#16531 = VERTEX_POINT ( 'NONE', #21054 ) ;
#16532 = ORIENTED_EDGE ( 'NONE', *, *, #1716, .T. ) ;
#16533 = CARTESIAN_POINT ( 'NONE',  ( -74.16669567121724072, 95.38686586275396451, 79.68462973531357818 ) ) ;
#16534 = AXIS2_PLACEMENT_3D ( 'NONE', #11821, #13655, #8343 ) ;
#16535 = PRODUCT ( 'Moving Jaw', 'Moving Jaw', '', ( #15297 ) ) ;
#16536 = PLANE ( 'NONE',  #19134 ) ;
#16537 = EDGE_CURVE ( 'NONE', #17163, #7184, #13287, .T. ) ;
#16538 = CONTEXT_DEPENDENT_SHAPE_REPRESENTATION ( #7208, #9012 ) ;
#16539 =( GEOMETRIC_REPRESENTATION_CONTEXT ( 3 ) GLOBAL_UNCERTAINTY_ASSIGNED_CONTEXT ( ( #15711 ) ) GLOBAL_UNIT_ASSIGNED_CONTEXT ( ( #16234, #18058, #589 ) ) REPRESENTATION_CONTEXT ( 'NONE', 'WORKASPACE' ) );
#16540 = CARTESIAN_POINT ( 'NONE',  ( 79.99331838321626265, 54.99999999999999289, -6.033931352371312506 ) ) ;
#16541 = EDGE_CURVE ( 'NONE', #6907, #16237, #10842, .T. ) ;
#16542 = AXIS2_PLACEMENT_3D ( 'NONE', #19374, #11121, #3969 ) ;
#16543 = DIRECTION ( 'NONE',  ( 1.000000000000000000, 0.000000000000000000, -1.386679829960243376E-14 ) ) ;
#16544 = ORIENTED_EDGE ( 'NONE', *, *, #21272, .T. ) ;
#16545 = CARTESIAN_POINT ( 'NONE',  ( 40.93042701181084908, 108.3156947416822362, 71.72688916598494302 ) ) ;
#16546 = CARTESIAN_POINT ( 'NONE',  ( -14.00607518686419084, 180.2131691732588195, 308.7767599486462586 ) ) ;
#16547 = ORIENTED_EDGE ( 'NONE', *, *, #6196, .F. ) ;
#16548 = LINE ( 'NONE', #7799, #1550 ) ;
#16549 = VERTEX_POINT ( 'NONE', #17403 ) ;
#16550 = CARTESIAN_POINT ( 'NONE',  ( -164.0000000000000000, 1.999999999999998224, -7.999999999999979572 ) ) ;
#16551 = FACE_OUTER_BOUND ( 'NONE', #5901, .T. ) ;
#16553 = B_SPLINE_CURVE_WITH_KNOTS ( 'NONE', 3,
 ( #19292, #20785, #5041, #12074, #19062, #11930, #1258, #6841, #13863, #4554, #18580, #10087, #8446, #15602, #8246, #4768, #15495, #22446 ),
 .UNSPECIFIED., .F., .F.,
 ( 4, 2, 2, 2, 2, 2, 2, 2, 4 ),
 ( 0.000000000000000000, 0.1250000000000000000, 0.2500000000000000000, 0.3750000000000000000, 0.5000000000000000000, 0.6250000000000000000, 0.7500000000000000000, 0.8750000000000000000, 1.000000000000000000 ),
 .UNSPECIFIED. ) ;
#16552 = CARTESIAN_POINT ( 'NONE',  ( -17.94552162158367281, 88.10632231613314502, 77.37285291568925061 ) ) ;
#16554 = AXIS2_PLACEMENT_3D ( 'NONE', #18667, #2933, #9949 ) ;
#16555 = ORIENTED_EDGE ( 'NONE', *, *, #17533, .F. ) ;
#16556 = EDGE_CURVE ( 'NONE', #15942, #16446, #2101, .T. ) ;
#16557 = AXIS2_PLACEMENT_3D ( 'NONE', #19994, #5873, #19655 ) ;
#16558 = ADVANCED_FACE ( 'NONE', ( #15679 ), #15794, .F. ) ;
#16559 = CARTESIAN_POINT ( 'NONE',  ( 1.364375150383346228E-14, 45.00000000000000000, -9.836439021161248541E-15 ) ) ;
#16560 = AXIS2_PLACEMENT_3D ( 'NONE', #2158, #15745, #15866 ) ;
#16561 = EDGE_CURVE ( 'NONE', #7475, #5531, #15916, .T. ) ;
#16562 = CARTESIAN_POINT ( 'NONE',  ( -1.885502603235176489, 82.00000000000000000, -81.01068473295497085 ) ) ;
#16563 = AXIS2_PLACEMENT_3D ( 'NONE', #15701, #12015, #16985 ) ;
#16564 = EDGE_LOOP ( 'NONE', ( #20027, #20819, #10261, #18493 ) ) ;
#16565 = DIRECTION ( 'NONE',  ( 0.1337561903331546953, 0.9909881666746205298, -0.007192708699472573526 ) ) ;
#16566 = CARTESIAN_POINT ( 'NONE',  ( -89.35684609684774671, 89.12360481520539679, 51.47532503655791913 ) ) ;
#16567 = EDGE_CURVE ( 'NONE', #4308, #12773, #13644, .T. ) ;
#16568 = VERTEX_POINT ( 'NONE', #14190 ) ;
#16569 = LINE ( 'NONE', #13112, #3245 ) ;
#16570 = AXIS2_PLACEMENT_3D ( 'NONE', #5096, #18900, #22440 ) ;
#16571 = CARTESIAN_POINT ( 'NONE',  ( -51.19659413568783890, 110.8744609730857178, -46.41152423219341472 ) ) ;
#16572 = EDGE_CURVE ( 'NONE', #19973, #22152, #16231, .T. ) ;
#16573 = ORIENTED_EDGE ( 'NONE', *, *, #3343, .T. ) ;
#16574 = DIRECTION ( 'NONE',  ( -0.01292394549866727679, -0.005513023399720742325, -0.9999012842304692006 ) ) ;
#16575 = TOROIDAL_SURFACE ( 'NONE', #5902, 26.23296215977915935, 2.000000000000000000 ) ;
#16576 = DIRECTION ( 'NONE',  ( 0.9999164797902015955, 6.965998958219364448E-18, -0.01292414190464157182 ) ) ;
#16577 = ORIENTED_EDGE ( 'NONE', *, *, #14419, .T. ) ;
#16578 = EDGE_CURVE ( 'NONE', #19228, #7484, #13273, .T. ) ;
#16579 = FACE_OUTER_BOUND ( 'NONE', #2100, .T. ) ;
#16580 = CARTESIAN_POINT ( 'NONE',  ( -36.94244151028510004, 91.99797716581188922, 84.44721085690417794 ) ) ;
#16581 = ORIENTED_EDGE ( 'NONE', *, *, #9630, .F. ) ;
#16582 = CARTESIAN_POINT ( 'NONE',  ( -69.72166291831146623, 97.03531796885383187, 80.87252918713471672 ) ) ;
#16583 = TOROIDAL_SURFACE ( 'NONE', #13258, 10.00000000000000355, 2.000000000000000000 ) ;
#16584 = ORIENTED_EDGE ( 'NONE', *, *, #21082, .T. ) ;
#16585 = CARTESIAN_POINT ( 'NONE',  ( -45.96195738621045024, 164.6879759653328961, -74.13402305205957532 ) ) ;
#16586 = CARTESIAN_POINT ( 'NONE',  ( 3.457270245634818995, 81.64368954560634961, -98.46779458785447048 ) ) ;
#16587 = CARTESIAN_POINT ( 'NONE',  ( -55.33804461215960657, 114.2193244133317904, 167.6379947637574617 ) ) ;
#16588 = CARTESIAN_POINT ( 'NONE',  ( -164.0000000000000000, 20.00000000000000000, 4.016841501203319170E-14 ) ) ;
#16589 = EDGE_CURVE ( 'NONE', #10697, #12374, #20934, .T. ) ;
#16590 = ORIENTED_EDGE ( 'NONE', *, *, #15484, .F. ) ;
#16591 = CARTESIAN_POINT ( 'NONE',  ( -1.386679829960242619E-13, 18.00000000000000355, -9.999999999999994671 ) ) ;
#16592 = DIRECTION ( 'NONE',  ( -0.000000000000000000, -1.000000000000000000, -0.000000000000000000 ) ) ;
#16593 = CARTESIAN_POINT ( 'NONE',  ( -50.86956732378053658, 110.1619587132339717, -46.15522227794017596 ) ) ;
#16594 = ORIENTED_EDGE ( 'NONE', *, *, #5452, .F. ) ;
#16595 = VECTOR ( 'NONE', #18982, 1000.000000000000000 ) ;
#16596 = CARTESIAN_POINT ( 'NONE',  ( -68.71681667565952978, 91.17157287525388654, 85.89527988174785378 ) ) ;
#16597 = VERTEX_POINT ( 'NONE', #7043 ) ;
#16598 = CIRCLE ( 'NONE', #16948, 4.500000000000006217 ) ;
#16599 = ORIENTED_EDGE ( 'NONE', *, *, #10816, .T. ) ;
#16600 = CARTESIAN_POINT ( 'NONE',  ( -84.54548942822992785, 75.02649460866172149, 3.357556456965392844 ) ) ;
#16601 = CARTESIAN_POINT ( 'NONE',  ( -90.10787854355197624, 88.43547347757348120, 52.79927570075625454 ) ) ;
#16602 = AXIS2_PLACEMENT_3D ( 'NONE', #19816, #4086, #20155 ) ;
#16603 = CARTESIAN_POINT ( 'NONE',  ( -50.56692998826083851, 113.4816418249608034, -43.53918672598639716 ) ) ;
#16604 = ORIENTED_EDGE ( 'NONE', *, *, #19718, .T. ) ;
#16605 = EDGE_CURVE ( 'NONE', #6576, #18453, #5308, .T. ) ;
#16606 = EDGE_CURVE ( 'NONE', #5416, #15344, #3701, .T. ) ;
#16607 = CARTESIAN_POINT ( 'NONE',  ( -71.57732418163384125, 97.94802198267763060, 79.98373377021528086 ) ) ;
#16608 = DIRECTION ( 'NONE',  ( -0.01292394549866632963, -0.005513023399716958026, -0.9999012842304692006 ) ) ;
#16609 = AXIS2_PLACEMENT_3D ( 'NONE', #5493, #19174, #3448 ) ;
#16610 = CARTESIAN_POINT ( 'NONE',  ( -92.90824731599330732, 79.04398536104955042, -26.22411128322386631 ) ) ;
#16611 = DIRECTION ( 'NONE',  ( 0.01292394549866738782, 0.005513023399720700692, 0.9999012842304693116 ) ) ;
#16612 = CARTESIAN_POINT ( 'NONE',  ( 68.70320840996379275, 69.99999999999998579, 85.90686588605385055 ) ) ;
#16613 = ORIENTED_EDGE ( 'NONE', *, *, #3112, .F. ) ;
#16614 = ORIENTED_EDGE ( 'NONE', *, *, #16474, .F. ) ;
#16615 = DIRECTION ( 'NONE',  ( 0.9999164797902015955, 6.965998958219364448E-18, -0.01292414190464157182 ) ) ;
#16616 = DIRECTION ( 'NONE',  ( 0.8608023089638390246, -0.002744228680570686644, -0.5089320721780777879 ) ) ;
#16617 = VECTOR ( 'NONE', #17949, 1000.000000000000114 ) ;
#16618 = CARTESIAN_POINT ( 'NONE',  ( 18.67701816413673654, 183.9365283982369021, 318.2129698699529285 ) ) ;
#16619 = DIRECTION ( 'NONE',  ( 0.01292394549866740169, 0.005513023399720822990, 0.9999012842304693116 ) ) ;
#16620 = DIRECTION ( 'NONE',  ( 0.8981428216242087759, 0.000000000000000000, -0.4397038457472309259 ) ) ;
#16621 = ORIENTED_EDGE ( 'NONE', *, *, #6144, .T. ) ;
#16622 = AXIS2_PLACEMENT_3D ( 'NONE', #2085, #7353, #9066 ) ;
#16623 = CARTESIAN_POINT ( 'NONE',  ( 0.000000000000000000, 0.000000000000000000, 0.000000000000000000 ) ) ;
#16624 = DIRECTION ( 'NONE',  ( -0.01292394549866741904, -0.005513023399721091004, -0.9999012842304693116 ) ) ;
#16625 = ORIENTED_EDGE ( 'NONE', *, *, #13317, .F. ) ;
#16626 = FACE_OUTER_BOUND ( 'NONE', #5566, .T. ) ;
#16627 = EDGE_LOOP ( 'NONE', ( #11120, #17870, #1126 ) ) ;
#16628 = CIRCLE ( 'NONE', #3014, 93.00000000000001421 ) ;
#16629 = CARTESIAN_POINT ( 'NONE',  ( 41.17443399381281921, 107.5575245709146941, 71.06985290734100147 ) ) ;
#16630 = ORIENTED_EDGE ( 'NONE', *, *, #2356, .F. ) ;
#16631 = EDGE_CURVE ( 'NONE', #13286, #848, #18408, .T. ) ;
#16632 = AXIS2_PLACEMENT_3D ( 'NONE', #21694, #9775, #2430 ) ;
#16633 = LINE ( 'NONE', #6149, #6621 ) ;
#16634 = DIRECTION ( 'NONE',  ( 0.8981428216242030027, 0.000000000000000000, 0.4397038457472430273 ) ) ;
#16635 = FACE_OUTER_BOUND ( 'NONE', #8507, .T. ) ;
#16636 = CARTESIAN_POINT ( 'NONE',  ( 40.57355171551004247, 108.0982075334647163, 198.8652726751216733 ) ) ;
#16637 = CYLINDRICAL_SURFACE ( 'NONE', #321, 9.999999999999998224 ) ;
#16638 = CARTESIAN_POINT ( 'NONE',  ( -64.22027802397437313, 106.9149828242082947, 60.74567061489647557 ) ) ;
#16639 = VERTEX_POINT ( 'NONE', #2333 ) ;
#16640 = DIRECTION ( 'NONE',  ( 7.125109674160258889E-05, -0.9999848031710252272, 0.005512562950849897447 ) ) ;
#16641 = DIRECTION ( 'NONE',  ( 1.000000000000000000, 0.000000000000000000, 0.000000000000000000 ) ) ;
#16642 = CARTESIAN_POINT ( 'NONE',  ( 88.91001978040560516, 99.16808946942325065, -64.76993003646445857 ) ) ;
#16643 = AXIS2_PLACEMENT_3D ( 'NONE', #221, #7217, #17923 ) ;
#16644 = CARTESIAN_POINT ( 'NONE',  ( -164.0000000000000000, 20.00000000000000000, -53.76161406891256433 ) ) ;
#16645 = CIRCLE ( 'NONE', #5223, 3.999999999999995559 ) ;
#16646 = CARTESIAN_POINT ( 'NONE',  ( 91.85126960211910330, 79.84876637418037149, -31.24149931482740783 ) ) ;
#16647 = CARTESIAN_POINT ( 'NONE',  ( -9.712210512681874519, 187.7615446298876236, 321.1679357793473173 ) ) ;
#16648 = LINE ( 'NONE', #11450, #12592 ) ;
#16649 = ORIENTED_EDGE ( 'NONE', *, *, #8921, .F. ) ;
#16650 = CARTESIAN_POINT ( 'NONE',  ( 50.26215390436148311, 189.4880035784398160, -93.58148208147835589 ) ) ;
#16651 = CARTESIAN_POINT ( 'NONE',  ( 64.31784532510161512, 144.7109461922390778, -53.19707257213011076 ) ) ;
#16652 = CARTESIAN_POINT ( 'NONE',  ( -13.42494546845840020, 180.9759964141439923, 309.9922123620679031 ) ) ;
#16653 = EDGE_LOOP ( 'NONE', ( #13885, #18295, #18921, #11475 ) ) ;
#16654 = ORIENTED_EDGE ( 'NONE', *, *, #15691, .F. ) ;
#16655 = CARTESIAN_POINT ( 'NONE',  ( -63.92222308695259869, 94.02752048664899576, 83.80561885825630952 ) ) ;
#16656 = VECTOR ( 'NONE', #13511, 1000.000000000000000 ) ;
#16657 = AXIS2_PLACEMENT_3D ( 'NONE', #1838, #17714, #13802 ) ;
#16658 = DIRECTION ( 'NONE',  ( 0.01292394549866727679, 0.005513023399720742325, 0.9999012842304692006 ) ) ;
#16659 = EDGE_CURVE ( 'NONE', #7484, #4883, #9436, .T. ) ;
#16660 = CARTESIAN_POINT ( 'NONE',  ( 1.721625266288820955, 45.00000000000000000, 109.9865264768483968 ) ) ;
#16661 = AXIS2_PLACEMENT_3D ( 'NONE', #17418, #9108, #2012 ) ;
#16662 = ORIENTED_EDGE ( 'NONE', *, *, #20733, .F. ) ;
#16663 = CARTESIAN_POINT ( 'NONE',  ( 12.05007958101849574, 187.6699938018584533, 304.8922276890921239 ) ) ;
#16664 = CARTESIAN_POINT ( 'NONE',  ( 83.82126922308901840, 105.0000000000000000, -71.23197895489381892 ) ) ;
#16665 = VERTEX_POINT ( 'NONE', #7502 ) ;
#16666 = DIRECTION ( 'NONE',  ( -7.125109674118361251E-05, 0.9999848031710253382, -0.005512562950849477644 ) ) ;
#16667 = CARTESIAN_POINT ( 'NONE',  ( 0.000000000000000000, 0.000000000000000000, 0.000000000000000000 ) ) ;
#16668 = DIRECTION ( 'NONE',  ( -7.125109674381882011E-05, 0.9999848031710253382, -0.005512562950849702291 ) ) ;
#16669 = AXIS2_PLACEMENT_3D ( 'NONE', #17609, #3808, #19200 ) ;
#16670 = ORIENTED_EDGE ( 'NONE', *, *, #20741, .F. ) ;
#16671 = CIRCLE ( 'NONE', #7848, 8.000000000000014211 ) ;
#16672 = ADVANCED_FACE ( 'NONE', ( #14531 ), #22044, .T. ) ;
#16673 = ORIENTED_EDGE ( 'NONE', *, *, #15548, .F. ) ;
#16674 = CARTESIAN_POINT ( 'NONE',  ( 164.0000000000000000, 1.999999999999998224, 2.250243343269062756E-12 ) ) ;
#16675 = CARTESIAN_POINT ( 'NONE',  ( -84.07537730384211727, 105.0000000000000000, -70.09082476868248079 ) ) ;
#16676 = ADVANCED_FACE ( 'NONE', ( #5757 ), #4153, .T. ) ;
#16677 = ORIENTED_EDGE ( 'NONE', *, *, #16410, .T. ) ;
#16678 = VECTOR ( 'NONE', #8377, 999.9999999999998863 ) ;
#16679 = AXIS2_PLACEMENT_3D ( 'NONE', #6874, #14021, #17824 ) ;
#16680 = UNCERTAINTY_MEASURE_WITH_UNIT (LENGTH_MEASURE( 1.000000000000000082E-05 ), #5156, 'distance_accuracy_value', 'NONE');
#16681 = CARTESIAN_POINT ( 'NONE',  ( -39.24016587203285411, 108.3652131041115467, 59.04542680541619859 ) ) ;
#16682 = CARTESIAN_POINT ( 'NONE',  ( -89.07090003446140258, 88.54756155696802011, 50.44072191361355806 ) ) ;
#16683 = PRODUCT_CONTEXT ( 'NONE', #3084, 'mechanical' ) ;
#16684 = VECTOR ( 'NONE', #21527, 1000.000000000000114 ) ;
#16685 = ADVANCED_FACE ( 'NONE', ( #8385 ), #6562, .F. ) ;
#16686 = ORIENTED_EDGE ( 'NONE', *, *, #5120, .F. ) ;
#16687 = ADVANCED_FACE ( 'NONE', ( #18525 ), #22168, .T. ) ;
#16688 = CIRCLE ( 'NONE', #13373, 3.399999999999986144 ) ;
#16689 = DIRECTION ( 'NONE',  ( 0.9726991065672921932, 0.2316562896908778701, -0.01384960395994898341 ) ) ;
#16690 = EDGE_CURVE ( 'NONE', #22542, #17948, #7035, .T. ) ;
#16691 = CARTESIAN_POINT ( 'NONE',  ( -50.82071652507229231, 109.9724431479075832, -46.08693180671795631 ) ) ;
#16692 = CARTESIAN_POINT ( 'NONE',  ( 13.18210494705709301, 190.2238003902018875, 320.8376354884886723 ) ) ;
#16693 = CARTESIAN_POINT ( 'NONE',  ( -41.37799937016134777, 161.8891746470816884, 277.2055869492696161 ) ) ;
#16694 = CARTESIAN_POINT ( 'NONE',  ( -154.0000000000000000, 18.00000000000000355, 53.76161406891259986 ) ) ;
#16695 = EDGE_CURVE ( 'NONE', #10082, #14514, #19834, .T. ) ;
#16696 = DIRECTION ( 'NONE',  ( 0.000000000000000000, 1.000000000000000000, -0.000000000000000000 ) ) ;
#16697 = CARTESIAN_POINT ( 'NONE',  ( -38.46706438352712354, 91.17157287525387233, 85.27439087629284131 ) ) ;
#16698 = ORIENTED_EDGE ( 'NONE', *, *, #6977, .F. ) ;
#16699 = CARTESIAN_POINT ( 'NONE',  ( -154.0000000000000000, 18.00000000000000355, -53.76161406891256433 ) ) ;
#16700 = ORIENTED_EDGE ( 'NONE', *, *, #9282, .T. ) ;
#16701 = CARTESIAN_POINT ( 'NONE',  ( -41.47069032946998846, 166.0668615304125808, 273.1833561390217824 ) ) ;
#16702 = CARTESIAN_POINT ( 'NONE',  ( -88.81160319069240927, 71.93448555257867838, 64.93693744786097000 ) ) ;
#16703 = CARTESIAN_POINT ( 'NONE',  ( -3.227672524189195702, 173.4898748461659750, 324.6532631065690566 ) ) ;
#16704 = CARTESIAN_POINT ( 'NONE',  ( -8.474913151513398191, 165.2748993292589148, 308.3080180880245962 ) ) ;
#16705 = EDGE_CURVE ( 'NONE', #21379, #13316, #14011, .T. ) ;
#16706 = AXIS2_PLACEMENT_3D ( 'NONE', #6934, #9947, #18999 ) ;
#16707 = EDGE_LOOP ( 'NONE', ( #8274, #1015, #15055, #10995 ) ) ;
#16708 = CIRCLE ( 'NONE', #2008, 10.71774939102741264 ) ;
#16709 = EDGE_CURVE ( 'NONE', #17159, #11064, #8136, .T. ) ;
#16710 = CARTESIAN_POINT ( 'NONE',  ( 1.307423968679454873, 137.5572120012638777, 101.1529262059483045 ) ) ;
#16711 = EDGE_CURVE ( 'NONE', #18167, #20021, #10131, .T. ) ;
#16712 = VERTEX_POINT ( 'NONE', #17139 ) ;
#16713 = ORIENTED_EDGE ( 'NONE', *, *, #14129, .T. ) ;
#16714 = CARTESIAN_POINT ( 'NONE',  ( -88.16253418885003157, 88.15973640631176522, 52.99065010345115923 ) ) ;
#16715 = AXIS2_PLACEMENT_3D ( 'NONE', #18190, #12561, #17864 ) ;
#16716 = VERTEX_POINT ( 'NONE', #9898 ) ;
#16717 = ADVANCED_FACE ( 'NONE', ( #13806 ), #15430, .F. ) ;
#16718 = ADVANCED_FACE ( 'NONE', ( #11738 ), #6461, .F. ) ;
#16719 = DIRECTION ( 'NONE',  ( 0.000000000000000000, 0.000000000000000000, 1.000000000000000000 ) ) ;
#16720 = CARTESIAN_POINT ( 'NONE',  ( 17.45193422578444142, 176.6200190940306527, 112.2300147490413167 ) ) ;
#16721 = DIRECTION ( 'NONE',  ( 1.000000000000000000, 0.000000000000000000, 1.362186893977296347E-14 ) ) ;
#16722 = CARTESIAN_POINT ( 'NONE',  ( -38.19275834114522894, 94.78920923681313582, 83.58418063251983199 ) ) ;
#16723 = ORIENTED_EDGE ( 'NONE', *, *, #9480, .T. ) ;
#16724 = DIRECTION ( 'NONE',  ( 0.9999164797902015955, 6.965998958219364448E-18, -0.01292414190464157182 ) ) ;
#16725 = CARTESIAN_POINT ( 'NONE',  ( 54.52327687265665190, 2.000000000000000000, 111.3697098814019029 ) ) ;
#16726 = CARTESIAN_POINT ( 'NONE',  ( 19.87237553197154938, 182.8168944290782179, 318.2233073528176419 ) ) ;
#16727 = FACE_OUTER_BOUND ( 'NONE', #12946, .T. ) ;
#16728 = DIRECTION ( 'NONE',  ( 2.025474946048326158E-22, -1.000000000000000000, 1.876735158486679638E-22 ) ) ;
#16729 = AXIS2_PLACEMENT_3D ( 'NONE', #16226, #4115, #12998 ) ;
#16730 = ADVANCED_FACE ( 'NONE', ( #11971 ), #22268, .T. ) ;
#16731 = CARTESIAN_POINT ( 'NONE',  ( -68.69096839185023384, 72.00000000000000000, 87.89511284132827029 ) ) ;
#16732 = DIRECTION ( 'NONE',  ( -7.125109674403838460E-05, 0.9999848031710254492, -0.005512562950847868688 ) ) ;
#16733 = ORIENTED_EDGE ( 'NONE', *, *, #3358, .T. ) ;
#16734 = DIRECTION ( 'NONE',  ( 0.01292394549866738608, 0.005513023399720699824, 0.9999012842304692006 ) ) ;
#16735 = EDGE_LOOP ( 'NONE', ( #3016, #20638, #4527, #16739 ) ) ;
#16736 = CARTESIAN_POINT ( 'NONE',  ( 5.047586898063077143, 159.3382231987902173, 324.6243296352952825 ) ) ;
#16737 = CARTESIAN_POINT ( 'NONE',  ( -41.15169610061244754, 101.1708071963161615, 65.90309081746964637 ) ) ;
#16738 = VERTEX_POINT ( 'NONE', #4701 ) ;
#16739 = ORIENTED_EDGE ( 'NONE', *, *, #21404, .F. ) ;
#16740 = EDGE_CURVE ( 'NONE', #2396, #17033, #4796, .T. ) ;
#16741 = CARTESIAN_POINT ( 'NONE',  ( 42.04378466868516995, 168.6907664596096765, 34.06594930769865925 ) ) ;
#16742 = CARTESIAN_POINT ( 'NONE',  ( -89.96695160930070756, 69.55454869655315520, 63.52358046848883077 ) ) ;
#16743 = AXIS2_PLACEMENT_3D ( 'NONE', #8035, #18836, #2769 ) ;
#16744 = CARTESIAN_POINT ( 'NONE',  ( -39.99665919160808869, 170.0000000000000284, 0.5169656761856410432 ) ) ;
#16745 = DIRECTION ( 'NONE',  ( 5.440186201345738641E-18, 1.000000000000000000, 1.334940939666364181E-17 ) ) ;
#16746 = ORIENTED_EDGE ( 'NONE', *, *, #15352, .F. ) ;
#16747 = CARTESIAN_POINT ( 'NONE',  ( -69.33518156588185377, 92.50622784628016859, 85.39700225480589779 ) ) ;
#16748 = CARTESIAN_POINT ( 'NONE',  ( 85.73191996558125538, 0.1220636790436879782, 21.03437761588512345 ) ) ;
#16749 = CARTESIAN_POINT ( 'NONE',  ( -71.30986567784941599, 88.03842148812331914, 69.24871475584893687 ) ) ;
#16750 = DIRECTION ( 'NONE',  ( -0.01104128644981183967, -0.5197558313507629757, -0.8542435049623791077 ) ) ;
#16751 = CARTESIAN_POINT ( 'NONE',  ( 89.40066202591057731, 79.46807343418986136, -29.95041408108882308 ) ) ;
#16752 = LINE ( 'NONE', #1000, #69 ) ;
#16753 = DIRECTION ( 'NONE',  ( 0.000000000000000000, 0.000000000000000000, 1.000000000000000000 ) ) ;
#16754 = ORIENTED_EDGE ( 'NONE', *, *, #5040, .F. ) ;
#16755 = DIRECTION ( 'NONE',  ( -5.440186201345738641E-18, -1.000000000000000000, -1.334940939666364181E-17 ) ) ;
#16756 = VERTEX_POINT ( 'NONE', #22048 ) ;
#16757 = ADVANCED_FACE ( 'NONE', ( #15540 ), #6351, .T. ) ;
#16758 = CARTESIAN_POINT ( 'NONE',  ( -40.94831321612058161, 169.5761513248267818, 277.1576504944517296 ) ) ;
#16759 = CARTESIAN_POINT ( 'NONE',  ( -14.07499434214214240, 182.1903141478447310, 310.6856384327238629 ) ) ;
#16760 = EDGE_CURVE ( 'NONE', #8927, #6699, #22062, .T. ) ;
#16761 = ORIENTED_EDGE ( 'NONE', *, *, #9993, .T. ) ;
#16762 = ORIENTED_EDGE ( 'NONE', *, *, #16953, .T. ) ;
#16763 = CARTESIAN_POINT ( 'NONE',  ( -109.9908127769221693, 169.9999999999999716, 1.421655609510535045 ) ) ;
#16764 = PRODUCT_RELATED_PRODUCT_CATEGORY ( 'part', '', ( #8650 ) ) ;
#16765 = CARTESIAN_POINT ( 'NONE',  ( 22.08632752877390715, 147.9377667753725802, 276.4622185031857384 ) ) ;
#16766 = CARTESIAN_POINT ( 'NONE',  ( 3.833582208902202471, 166.6352317792378415, 296.5970240496424708 ) ) ;
#16767 = ORIENTED_EDGE ( 'NONE', *, *, #11932, .F. ) ;
#16768 = DIRECTION ( 'NONE',  ( -0.9999164797902015955, -8.506845633049208051E-18, 0.01292414190464159611 ) ) ;
#16769 = DIRECTION ( 'NONE',  ( -0.01292394549866695240, -0.005513023399725255208, -0.9999012842304693116 ) ) ;
#16770 = EDGE_LOOP ( 'NONE', ( #11670, #4161 ) ) ;
#16771 = ORIENTED_EDGE ( 'NONE', *, *, #19305, .T. ) ;
#16772 = CARTESIAN_POINT ( 'NONE',  ( -106.5693380255448517, 79.05027630924986681, -27.25937202119003189 ) ) ;
#16773 = VECTOR ( 'NONE', #3909, 1000.000000000000114 ) ;
#16774 = LINE ( 'NONE', #1142, #8232 ) ;
#16775 = DIRECTION ( 'NONE',  ( -0.3101392564284313758, -0.9506461370142479383, 0.009250070373107143265 ) ) ;
#16776 = ORIENTED_EDGE ( 'NONE', *, *, #6717, .F. ) ;
#16777 = EDGE_CURVE ( 'NONE', #5296, #7668, #1186, .T. ) ;
#16778 = DIRECTION ( 'NONE',  ( -0.006350819331213228454, 0.8709385446395345731, -0.4913509118287984201 ) ) ;
#16779 = CARTESIAN_POINT ( 'NONE',  ( 38.46706438352716617, 69.99999999999998579, -85.27439087629286973 ) ) ;
#16780 = VERTEX_POINT ( 'NONE', #17040 ) ;
#16781 = FACE_OUTER_BOUND ( 'NONE', #5132, .T. ) ;
#16782 = CARTESIAN_POINT ( 'NONE',  ( -35.42010074854528767, 108.0982075334647163, 199.8475074598744357 ) ) ;
#16783 = ADVANCED_BREP_SHAPE_REPRESENTATION ( '', ( #1836, #6292 ), #11807 ) ;
#16784 = SHAPE_DEFINITION_REPRESENTATION ( #17686, #10182 ) ;
#16785 = VERTEX_POINT ( 'NONE', #1305 ) ;
#16786 = ADVANCED_FACE ( 'NONE', ( #8287 ), #15320, .F. ) ;
#16787 = CARTESIAN_POINT ( 'NONE',  ( 90.42246537646656179, 78.26562148642793204, -32.93420195958647412 ) ) ;
#16788 = ORIENTED_EDGE ( 'NONE', *, *, #5913, .F. ) ;
#16789 = FACE_OUTER_BOUND ( 'NONE', #13191, .T. ) ;
#16790 = LINE ( 'NONE', #1038, #5208 ) ;
#16791 = DIRECTION ( 'NONE',  ( 0.9999164797902015955, 2.001050586450176109E-22, -0.01292414190464270113 ) ) ;
#16792 = DIRECTION ( 'NONE',  ( -0.01292394549866738608, -0.005513023399720699824, -0.9999012842304692006 ) ) ;
#16793 = EDGE_LOOP ( 'NONE', ( #21166, #17757, #9442, #15762 ) ) ;
#16794 = CARTESIAN_POINT ( 'NONE',  ( 35.37437755136402018, 92.78536193181560066, -83.65759506009361246 ) ) ;
#16795 = DIRECTION ( 'NONE',  ( -0.000000000000000000, -1.000000000000000000, -0.000000000000000000 ) ) ;
#16796 = ORIENTED_EDGE ( 'NONE', *, *, #19044, .F. ) ;
#16797 = LINE ( 'NONE', #20094, #11063 ) ;
#16798 = CARTESIAN_POINT ( 'NONE',  ( -10.81068638156953376, 113.7241309854131259, 131.6549996620339300 ) ) ;
#16799 = CARTESIAN_POINT ( 'NONE',  ( -10.39470828226744636, 145.5140731825025284, 276.5683172678064352 ) ) ;
#16800 = LINE ( 'NONE', #4597, #12848 ) ;
#16801 = AXIS2_PLACEMENT_3D ( 'NONE', #11009, #573, #19617 ) ;
#16802 = DIRECTION ( 'NONE',  ( -0.01292394549866741384, -0.005513023399720269613, -0.9999012842304692006 ) ) ;
#16803 = DIRECTION ( 'NONE',  ( 0.9232306267972772984, 1.069144893909150629E-19, -0.3842462878721229491 ) ) ;
#16804 = ADVANCED_FACE ( 'NONE', ( #3989, #8626 ), #16338, .T. ) ;
#16805 = ORIENTED_EDGE ( 'NONE', *, *, #1098, .T. ) ;
#16806 = DIRECTION ( 'NONE',  ( 0.01292394549866733230, 0.005513023399720419666, 0.9999012842304692006 ) ) ;
#16807 = ADVANCED_FACE ( 'NONE', ( #17930 ), #5719, .T. ) ;
#16808 = DIRECTION ( 'NONE',  ( 0.01292394549866705648, 0.005513023399720703294, 0.9999012842304692006 ) ) ;
#16809 = EDGE_LOOP ( 'NONE', ( #10805, #14377, #21929, #20566, #6009 ) ) ;
#16810 = ORIENTED_EDGE ( 'NONE', *, *, #18788, .T. ) ;
#16811 = CARTESIAN_POINT ( 'NONE',  ( -1.788039671088772931, 157.5463400564191545, 323.7224625657159436 ) ) ;
#16812 = CARTESIAN_POINT ( 'NONE',  ( -88.16339405475061142, 88.25449051743922269, 52.91957891188045693 ) ) ;
#16813 = ORIENTED_EDGE ( 'NONE', *, *, #17341, .T. ) ;
#16814 = AXIS2_PLACEMENT_3D ( 'NONE', #5492, #21128, #7335 ) ;
#16815 = EDGE_CURVE ( 'NONE', #984, #10132, #12840, .T. ) ;
#16816 = CARTESIAN_POINT ( 'NONE',  ( 65.93268019054301021, 104.4142135623730638, 71.73965483371370055 ) ) ;
#16817 = FACE_OUTER_BOUND ( 'NONE', #9287, .T. ) ;
#16818 = CARTESIAN_POINT ( 'NONE',  ( 68.30941429790007646, 191.4143309225247549, 255.6230893828509352 ) ) ;
#16819 = ORIENTED_EDGE ( 'NONE', *, *, #10688, .T. ) ;
#16820 = DIRECTION ( 'NONE',  ( 0.01292414190464133070, 0.000000000000000000, 0.9999164797902015955 ) ) ;
#16821 = DIRECTION ( 'NONE',  ( -0.01292394549866740343, -0.005513023399721215904, -0.9999012842304693116 ) ) ;
#16822 = CARTESIAN_POINT ( 'NONE',  ( -1.163172771417702478, 87.00000000000001421, -89.99248318111824574 ) ) ;
#16823 = ADVANCED_FACE ( 'NONE', ( #12100 ), #21556, .T. ) ;
#16824 = EDGE_LOOP ( 'NONE', ( #928, #5177, #940, #10882 ) ) ;
#16825 = LINE ( 'NONE', #1207, #4166 ) ;
#16826 = CARTESIAN_POINT ( 'NONE',  ( 19.38059109545055492, 183.2942308163235055, 317.1334150972197676 ) ) ;
#16827 = DIRECTION ( 'NONE',  ( -0.01292394549866731669, -0.005513023399720593139, -0.9999012842304692006 ) ) ;
#16828 = CIRCLE ( 'NONE', #14639, 3.399999999999986144 ) ;
#16829 = CARTESIAN_POINT ( 'NONE',  ( -6.716850738106426633, 144.4960990889537413, 277.1001543104694633 ) ) ;
#16830 = DIRECTION ( 'NONE',  ( 1.000000000000000000, 0.000000000000000000, 0.000000000000000000 ) ) ;
#16831 = PRESENTATION_LAYER_ASSIGNMENT (  '', '', ( #12042 ) ) ;
#16832 = EDGE_CURVE ( 'NONE', #20978, #5517, #10255, .T. ) ;
#16833 = DIRECTION ( 'NONE',  ( 0.01292414190464177652, 1.902755938799532355E-22, 0.9999164797902015955 ) ) ;
#16834 = CARTESIAN_POINT ( 'NONE',  ( -10.02114103959053182, 187.8727639482237635, 308.1601374225635368 ) ) ;
#16835 = VERTEX_POINT ( 'NONE', #18043 ) ;
#16836 = CARTESIAN_POINT ( 'NONE',  ( 3.943435745640934798, 166.6820924781355302, 305.0961849656022764 ) ) ;
#16837 = ORIENTED_EDGE ( 'NONE', *, *, #18628, .T. ) ;
#16838 = ORIENTED_EDGE ( 'NONE', *, *, #5883, .F. ) ;
#16839 = PLANE ( 'NONE',  #8592 ) ;
#16840 = VECTOR ( 'NONE', #22155, 1000.000000000000114 ) ;
#16841 = EDGE_LOOP ( 'NONE', ( #14930, #7946, #2680, #4783 ) ) ;
#16842 = AXIS2_PLACEMENT_3D ( 'NONE', #11902, #11667, #8318 ) ;
#16843 = CARTESIAN_POINT ( 'NONE',  ( 79.59047627986713280, 75.13699351169599083, -6.129150517636113626 ) ) ;
#16844 = CARTESIAN_POINT ( 'NONE',  ( -86.63143169152132828, 104.5954341936825642, -67.78689798060399596 ) ) ;
#16845 = CARTESIAN_POINT ( 'NONE',  ( 105.6047345086702052, 78.54962563481561233, -30.78394349069533575 ) ) ;
#16846 = DIRECTION ( 'NONE',  ( -0.01035335185279159971, -0.005513005182356926943, -0.9999312050732648283 ) ) ;
#16847 = EDGE_CURVE ( 'NONE', #17590, #1849, #9291, .T. ) ;
#16848 = CARTESIAN_POINT ( 'NONE',  ( -1.163172771417702700, 69.99999999999998579, -89.99248318111824574 ) ) ;
#16849 = FACE_OUTER_BOUND ( 'NONE', #9019, .T. ) ;
#16850 = CARTESIAN_POINT ( 'NONE',  ( 42.43719399169239637, 94.56237283683982753, 82.91753452609758313 ) ) ;
#16851 = CARTESIAN_POINT ( 'NONE',  ( -7.475646132950445555, 70.80384757729335377, -81.73701953211951832 ) ) ;
#16852 = DIRECTION ( 'NONE',  ( 0.01292394549866731149, 0.005513023399720593139, 0.9999012842304692006 ) ) ;
#16853 = CARTESIAN_POINT ( 'NONE',  ( 91.28310237474674693, 79.93543901797764306, -31.44354501024116999 ) ) ;
#16854 = CARTESIAN_POINT ( 'NONE',  ( 91.21019055468687498, 34.61572286322119396, 28.82359390673205723 ) ) ;
#16855 = ORIENTED_EDGE ( 'NONE', *, *, #3895, .T. ) ;
#16856 = DIRECTION ( 'NONE',  ( 0.01292394549866738782, 0.005513023399720700692, 0.9999012842304693116 ) ) ;
#16857 = VERTEX_POINT ( 'NONE', #17828 ) ;
#16858 = ADVANCED_FACE ( 'NONE', ( #17269 ), #5062, .T. ) ;
#16859 = ORIENTED_EDGE ( 'NONE', *, *, #14984, .F. ) ;
#16860 = DIRECTION ( 'NONE',  ( -0.6080604969667605664, -0.004419696743559108250, -0.7938783901261144971 ) ) ;
#16861 = CARTESIAN_POINT ( 'NONE',  ( -14.45874313190398297, 179.5722162953435088, 309.6207302340725391 ) ) ;
#16862 = CIRCLE ( 'NONE', #7666, 3.099999999999998757 ) ;
#16863 = EDGE_LOOP ( 'NONE', ( #10864, #18163 ) ) ;
#16864 = ORIENTED_EDGE ( 'NONE', *, *, #18428, .T. ) ;
#16865 = FACE_BOUND ( 'NONE', #9661, .T. ) ;
#16866 = AXIS2_PLACEMENT_3D ( 'NONE', #6273, #21525, #7638 ) ;
#16867 = VERTEX_POINT ( 'NONE', #16219 ) ;
#16868 = LINE ( 'NONE', #12024, #13336 ) ;
#16869 = VECTOR ( 'NONE', #18964, 1000.000000000000000 ) ;
#16870 = CARTESIAN_POINT ( 'NONE',  ( 21.59772782749408648, 147.6508209369730196, 276.4701158578107538 ) ) ;
#16871 = ADVANCED_FACE ( 'NONE', ( #1534 ), #15560, .T. ) ;
#16872 = EDGE_CURVE ( 'NONE', #18377, #8063, #1891, .T. ) ;
#16873 = AXIS2_PLACEMENT_3D ( 'NONE', #22131, #2754, #6531 ) ;
#16874 = DIRECTION ( 'NONE',  ( -7.125109674243555432E-05, 0.9999848031710253382, -0.005512562950850175003 ) ) ;
#16875 = ORIENTED_EDGE ( 'NONE', *, *, #10051, .T. ) ;
#16876 = CARTESIAN_POINT ( 'NONE',  ( 11.93152547184112322, 187.7152878153667643, 304.8830991845499625 ) ) ;
#16877 = CYLINDRICAL_SURFACE ( 'NONE', #1114, 2.000000000000004441 ) ;
#16878 = CARTESIAN_POINT ( 'NONE',  ( -79.99331838321612054, 55.00000000000000000, 1.033931352371344481 ) ) ;
#16879 = CARTESIAN_POINT ( 'NONE',  ( -38.68617183816869698, 163.9153776386440882, 273.1592279730091377 ) ) ;
#16880 = CYLINDRICAL_SURFACE ( 'NONE', #8491, 2.000000000000004441 ) ;
#16881 = EDGE_LOOP ( 'NONE', ( #6798, #22462, #3626, #16979, #15286 ) ) ;
#16882 = DIRECTION ( 'NONE',  ( -5.440186201345738641E-18, -1.000000000000000000, -1.334940939666364181E-17 ) ) ;
#16883 = EDGE_LOOP ( 'NONE', ( #5848, #13605, #18651, #11118 ) ) ;
#16884 = FACE_BOUND ( 'NONE', #16440, .T. ) ;
#16885 = CARTESIAN_POINT ( 'NONE',  ( 9.196690372329049623, 142.8086146031528187, 274.7267082784170498 ) ) ;
#16886 = CIRCLE ( 'NONE', #10267, 120.0000000000000142 ) ;
#16887 = CIRCLE ( 'NONE', #3295, 110.5324305509042233 ) ;
#16888 = CARTESIAN_POINT ( 'NONE',  ( -9.785137964318257886, 187.5706118828227318, 308.1235300825433683 ) ) ;
#16889 = CARTESIAN_POINT ( 'NONE',  ( 9.109368757775365921, 142.0951589094185579, 256.6601876722492648 ) ) ;
#16890 = ORIENTED_EDGE ( 'NONE', *, *, #16987, .F. ) ;
#16891 = CARTESIAN_POINT ( 'NONE',  ( 42.92324425022518852, 106.8061942917681790, 70.38450200964520320 ) ) ;
#16892 = FACE_OUTER_BOUND ( 'NONE', #17089, .T. ) ;
#16893 = ORIENTED_EDGE ( 'NONE', *, *, #511, .F. ) ;
#16894 = CARTESIAN_POINT ( 'NONE',  ( 90.59090487622921728, 77.87375801460383684, -32.35420311765523849 ) ) ;
#16895 = CARTESIAN_POINT ( 'NONE',  ( 15.92090764981139017, 188.3996504711684281, 320.0687762302596866 ) ) ;
#16896 = PLANE ( 'NONE',  #11403 ) ;
#16897 = DIRECTION ( 'NONE',  ( -0.9999164797902015955, -2.001050586450178695E-22, 0.01292414190464131335 ) ) ;
#16898 = AXIS2_PLACEMENT_3D ( 'NONE', #11083, #16728, #19781 ) ;
#16899 = CARTESIAN_POINT ( 'NONE',  ( 92.82229925712802299, 72.00000000000000000, -1.199748770783335861 ) ) ;
#16900 = PRODUCT_DEFINITION_SHAPE ( 'NONE', 'NONE',  #22677 ) ;
#16901 = CARTESIAN_POINT ( 'NONE',  ( 0.000000000000000000, 1.999999999999998224, 124.0000000000000000 ) ) ;
#16902 = AXIS2_PLACEMENT_3D ( 'NONE', #7260, #12449, #13832 ) ;
#16903 = DIRECTION ( 'NONE',  ( 0.000000000000000000, 0.000000000000000000, 1.000000000000000000 ) ) ;
#16904 = ORIENTED_EDGE ( 'NONE', *, *, #6514, .T. ) ;
#16905 = DIRECTION ( 'NONE',  ( 0.000000000000000000, 0.000000000000000000, 1.000000000000000000 ) ) ;
#16906 = CARTESIAN_POINT ( 'NONE',  ( 51.50086788761742440, 181.5071008296286266, 255.8949677505804061 ) ) ;
#16907 = ORIENTED_EDGE ( 'NONE', *, *, #1370, .T. ) ;
#16908 = FACE_OUTER_BOUND ( 'NONE', #6896, .T. ) ;
#16909 =( BOUNDED_CURVE ( )  B_SPLINE_CURVE ( 3, ( #7802, #9646, #4333, #21461 ),
 .UNSPECIFIED., .F., .T. ) 
 B_SPLINE_CURVE_WITH_KNOTS ( ( 4, 4 ),
 ( 3.141592653589793560, 4.712388980384689674 ),
 .UNSPECIFIED. ) 
 CURVE ( )  GEOMETRIC_REPRESENTATION_ITEM ( )  RATIONAL_B_SPLINE_CURVE ( ( 1.000000000000000000, 0.8047378541243650485, 0.8047378541243650485, 1.000000000000000000 ) ) 
 REPRESENTATION_ITEM ( '' )  );
#16910 = CARTESIAN_POINT ( 'NONE',  ( -87.60134834604855314, 73.86311199051665710, 66.55747971618217207 ) ) ;
#16911 = ORIENTED_EDGE ( 'NONE', *, *, #169, .F. ) ;
#16912 = DIRECTION ( 'NONE',  ( 0.8504393858994485633, -0.002839416958724378954, -0.5260653843604455870 ) ) ;
#16913 = FACE_BOUND ( 'NONE', #9397, .T. ) ;
#16914 = PLANE ( 'NONE',  #13695 ) ;
#16915 = CARTESIAN_POINT ( 'NONE',  ( -17.78132405376864966, 69.99999999999998579, -83.07604999942009272 ) ) ;
#16916 = AXIS2_PLACEMENT_3D ( 'NONE', #19239, #8657, #6508 ) ;
#16917 = ORIENTED_EDGE ( 'NONE', *, *, #10107, .F. ) ;
#16918 = CARTESIAN_POINT ( 'NONE',  ( 6.473302864968229819, 81.92452521006620714, -95.06675942850819183 ) ) ;
#16919 = CARTESIAN_POINT ( 'NONE',  ( 45.23671757199362986, 168.6025580852140138, 18.02358667753535926 ) ) ;
#16920 = VERTEX_POINT ( 'NONE', #12525 ) ;
#16921 = AXIS2_PLACEMENT_3D ( 'NONE', #5992, #4666, #1269 ) ;
#16922 = CARTESIAN_POINT ( 'NONE',  ( -41.59208321381909457, 91.17157287525390075, -84.46951292587610283 ) ) ;
#16923 = AXIS2_PLACEMENT_3D ( 'NONE', #15820, #10967, #12371 ) ;
#16924 = CARTESIAN_POINT ( 'NONE',  ( -88.16535734749170672, 88.44291595549381668, 52.74862968121699680 ) ) ;
#16925 = CIRCLE ( 'NONE', #19095, 2.000000000000001332 ) ;
#16926 = CARTESIAN_POINT ( 'NONE',  ( 11.35084583594941066, 176.0618768581043980, 299.4481834837243355 ) ) ;
#16927 = PLANE ( 'NONE',  #8579 ) ;
#16928 = ORIENTED_EDGE ( 'NONE', *, *, #2460, .T. ) ;
#16929 = FACE_OUTER_BOUND ( 'NONE', #14193, .T. ) ;
#16930 = CIRCLE ( 'NONE', #19826, 2.499999999999988010 ) ;
#16931 = LINE ( 'NONE', #8193, #1543 ) ;
#16932 = CYLINDRICAL_SURFACE ( 'NONE', #1429, 11.00000000000000178 ) ;
#16933 = ORIENTED_EDGE ( 'NONE', *, *, #22105, .T. ) ;
#16934 = DIRECTION ( 'NONE',  ( -0.01292394549866743465, -0.005513023399721021615, -0.9999012842304692006 ) ) ;
#16935 = ADVANCED_FACE ( 'NONE', ( #19516 ), #20242, .T. ) ;
#16936 = B_SPLINE_CURVE_WITH_KNOTS ( 'NONE', 3,
 ( #2342, #21499, #14309, #18204, #7613, #12798, #19772, #4047, #2452, #11072, #9447, #14651, #19447, #10733, #17762, #2006 ),
 .UNSPECIFIED., .F., .F.,
 ( 4, 2, 2, 2, 2, 2, 2, 4 ),
 ( -9.611261265246428336E-06, 0.0004115787608243976327, 0.0008327687829140417632, 0.001253958805003685568, 0.001675148827093329807, 0.002517528871272620237, 0.002938718893362260356, 0.003359908915451900908 ),
 .UNSPECIFIED. ) ;
#16937 = CARTESIAN_POINT ( 'NONE',  ( -89.22440607450261041, 80.22990097357060790, -29.93634654116231530 ) ) ;
#16938 = DIRECTION ( 'NONE',  ( 0.01292394549866738782, 0.005513023399720468239, 0.9999012842304692006 ) ) ;
#16939 = EDGE_LOOP ( 'NONE', ( #22388, #21414, #22496, #17911 ) ) ;
#16940 = ADVANCED_FACE ( 'NONE', ( #5955 ), #9857, .F. ) ;
#16941 = FACE_OUTER_BOUND ( 'NONE', #19334, .T. ) ;
#16942 = CARTESIAN_POINT ( 'NONE',  ( -88.04574633781018633, 72.16093070441274904, 62.02807968949604600 ) ) ;
#16943 = DIRECTION ( 'NONE',  ( 0.003413786507422414233, -0.9644842718275420390, 0.2641182225045781706 ) ) ;
#16944 = CARTESIAN_POINT ( 'NONE',  ( -40.94813932551373625, 95.97017003981163441, 82.42564028881616878 ) ) ;
#16945 = CONICAL_SURFACE ( 'NONE', #15828, 3.399999999999991918, 1.029744258676652313 ) ;
#16946 = CARTESIAN_POINT ( 'NONE',  ( 13.84903886101111681, 155.5756827379013885, 104.2918126654085853 ) ) ;
#16947 = DIRECTION ( 'NONE',  ( -0.9999164797902015955, -6.965998958219364448E-18, 0.01292414190464157182 ) ) ;
#16948 = AXIS2_PLACEMENT_3D ( 'NONE', #13244, #9676, #716 ) ;
#16949 = ADVANCED_FACE ( 'NONE', ( #13102 ), #686, .F. ) ;
#16950 = FACE_OUTER_BOUND ( 'NONE', #4010, .T. ) ;
#16951 = CIRCLE ( 'NONE', #19846, 23.67057332475409126 ) ;
#16952 = CARTESIAN_POINT ( 'NONE',  ( 3.212657888003040974, 175.3835135662012874, 324.5595797047259907 ) ) ;
#16953 = EDGE_CURVE ( 'NONE', #650, #17451, #3511, .T. ) ;
#16954 = EDGE_LOOP ( 'NONE', ( #356, #21759, #13037, #3683 ) ) ;
#16955 = CARTESIAN_POINT ( 'NONE',  ( -11.35185528768898600, 185.6292709456122907, 278.3409550216183561 ) ) ;
#16956 = ORIENTED_EDGE ( 'NONE', *, *, #6726, .T. ) ;
#16957 = ORIENTED_EDGE ( 'NONE', *, *, #8252, .T. ) ;
#16958 = CARTESIAN_POINT ( 'NONE',  ( -21.67182210555940358, 59.11803865240464262, -129.2164758598523235 ) ) ;
#16959 = ADVANCED_FACE ( 'NONE', ( #11356 ), #20603, .T. ) ;
#16960 = AXIS2_PLACEMENT_3D ( 'NONE', #12994, #21559, #19724 ) ;
#16961 = EDGE_LOOP ( 'NONE', ( #12402, #20497, #6304, #7453 ) ) ;
#16962 = AXIS2_PLACEMENT_3D ( 'NONE', #6919, #13940, #7262 ) ;
#16963 = DIRECTION ( 'NONE',  ( -0.9999164797902015955, -6.965998958219364448E-18, 0.01292414190464157182 ) ) ;
#16964 = CARTESIAN_POINT ( 'NONE',  ( -50.43108932508832964, 106.8786590446587184, 71.51684434343255248 ) ) ;
#16965 = DIRECTION ( 'NONE',  ( 0.1296504907605110779, 0.005475273188902231650, 0.9915446392518419971 ) ) ;
#16966 = VECTOR ( 'NONE', #21474, 1000.000000000000227 ) ;
#16967 = EDGE_CURVE ( 'NONE', #14037, #18877, #16548, .T. ) ;
#16968 = ADVANCED_FACE ( 'NONE', ( #18363 ), #19958, .T. ) ;
#16969 = CARTESIAN_POINT ( 'NONE',  ( 86.24279638190517971, 74.99999999999998579, -1.114707239275309014 ) ) ;
#16970 = LINE ( 'NONE', #1231, #16656 ) ;
#16971 = EDGE_CURVE ( 'NONE', #19627, #8399, #4225, .T. ) ;
#16972 = VECTOR ( 'NONE', #15328, 1000.000000000000114 ) ;
#16973 = DIRECTION ( 'NONE',  ( 0.01292394549866740169, 0.005513023399720822990, 0.9999012842304693116 ) ) ;
#16974 = CARTESIAN_POINT ( 'NONE',  ( 43.08423624159371457, 94.48610424851698042, 82.84014869562157912 ) ) ;
#16975 = CARTESIAN_POINT ( 'NONE',  ( -64.99457118636313169, 170.0000000000000284, 0.8400692238016805868 ) ) ;
#16976 = DIRECTION ( 'NONE',  ( 7.125109674160325297E-05, -0.9999848031710252272, 0.005512562950849327591 ) ) ;
#16977 = EDGE_CURVE ( 'NONE', #21004, #17590, #8138, .T. ) ;
#16978 = DIRECTION ( 'NONE',  ( -0.9999164797902015955, -4.476705744456268255E-15, 0.01292414190464141917 ) ) ;
#16979 = ORIENTED_EDGE ( 'NONE', *, *, #19853, .F. ) ;
#16980 = CARTESIAN_POINT ( 'NONE',  ( -79.99331838321612054, 54.99999999999999289, 1.033931352371344481 ) ) ;
#16981 = AXIS2_PLACEMENT_3D ( 'NONE', #21994, #8334, #22326 ) ;
#16982 =( GEOMETRIC_REPRESENTATION_CONTEXT ( 3 ) GLOBAL_UNCERTAINTY_ASSIGNED_CONTEXT ( ( #13004 ) ) GLOBAL_UNIT_ASSIGNED_CONTEXT ( ( #17328, #4901, #1474 ) ) REPRESENTATION_CONTEXT ( 'NONE', 'WORKASPACE' ) );
#16983 = EDGE_CURVE ( 'NONE', #10445, #8451, #12199, .T. ) ;
#16984 = ORIENTED_EDGE ( 'NONE', *, *, #15326, .F. ) ;
#16985 = DIRECTION ( 'NONE',  ( 0.3101392564284310982, 0.9506461370142479383, -0.009250070373107712254 ) ) ;
#16986 = CARTESIAN_POINT ( 'NONE',  ( -8.409519743373715883, 185.4801247956302745, 308.0432246570530310 ) ) ;
#16987 = EDGE_CURVE ( 'NONE', #21648, #5580, #11139, .T. ) ;
#16988 = ORIENTED_EDGE ( 'NONE', *, *, #10201, .T. ) ;
#16989 = CARTESIAN_POINT ( 'NONE',  ( -3.234480676511187980, 189.9413464613920723, 274.8561509274957757 ) ) ;
#16990 = VERTEX_POINT ( 'NONE', #6421 ) ;
#16991 = EDGE_CURVE ( 'NONE', #16780, #5580, #15619, .T. ) ;
#16992 = AXIS2_PLACEMENT_3D ( 'NONE', #16458, #705, #7698 ) ;
#16993 = CARTESIAN_POINT ( 'NONE',  ( -70.91392079944854743, 71.82437938702648239, -84.09052168258642723 ) ) ;
#16994 = CIRCLE ( 'NONE', #5963, 2.000000000000000000 ) ;
#16995 = AXIS2_PLACEMENT_3D ( 'NONE', #17965, #19758, #18290 ) ;
#16996 = DIRECTION ( 'NONE',  ( -0.01292414190464174703, 0.000000000000000000, -0.9999164797902015955 ) ) ;
#16997 = CARTESIAN_POINT ( 'NONE',  ( 14.77414660359919374, 144.4974462979978398, 275.7313215082337479 ) ) ;
#16998 = ADVANCED_FACE ( 'NONE', ( #22452 ), #17202, .T. ) ;
#16999 = DIRECTION ( 'NONE',  ( 0.9506868100732489557, -0.3101525256269085928, 0.000000000000000000 ) ) ;
#17000 = DIRECTION ( 'NONE',  ( 0.9999164797902017066, -4.906538733281754926E-15, -0.01292414190464131508 ) ) ;
#17001 = VECTOR ( 'NONE', #6299, 999.9999999999998863 ) ;
#17002 = CARTESIAN_POINT ( 'NONE',  ( -106.2089377515398780, 77.12912189496638860, -28.62973177816246206 ) ) ;
#17003 = CARTESIAN_POINT ( 'NONE',  ( -36.90283430563165723, 95.89798883583559075, 85.13120909300619132 ) ) ;
#17004 = CARTESIAN_POINT ( 'NONE',  ( 39.42082737383937996, 69.99999999999998579, -83.51645567887783272 ) ) ;
#17005 = VERTEX_POINT ( 'NONE', #4776 ) ;
#17006 = DIRECTION ( 'NONE',  ( -0.7220859686467110405, 0.6917813203664554544, 0.005518937903674876050 ) ) ;
#17007 = DIRECTION ( 'NONE',  ( 0.9999164797902017066, 6.965998958219365988E-18, -0.01292414190464157356 ) ) ;
#17008 = CARTESIAN_POINT ( 'NONE',  ( 64.42123688909094881, 144.7550503794368524, -45.19786229828635271 ) ) ;
#17009 = CIRCLE ( 'NONE', #10758, 2.000000000000004441 ) ;
#17010 = MANIFOLD_SOLID_BREP ( 'Stock-MAS-425-1', #9681 ) ;
#17011 = VECTOR ( 'NONE', #5104, 1000.000000000000114 ) ;
#17012 = CARTESIAN_POINT ( 'NONE',  ( -25.54600055714195506, 324.4124461427009010, 319.6189258610973525 ) ) ;
#17013 = EDGE_CURVE ( 'NONE', #10015, #4443, #17446, .T. ) ;
#17014 = DIRECTION ( 'NONE',  ( -0.2317097747526779827, 0.9727820773532231957, -0.002368599673008279193 ) ) ;
#17015 = CARTESIAN_POINT ( 'NONE',  ( -44.65237404513518271, 168.6466622724118452, 27.18596972279685531 ) ) ;
#17016 = DIRECTION ( 'NONE',  ( 0.9909299940865190504, -0.1338359446631136318, -0.01207007604876911971 ) ) ;
#17017 = CLOSED_SHELL ( 'NONE', ( #1907, #4576, #3043, #3025, #16450, #14818, #7304, #16096, #16058, #6281, #14731, #9797, #3648, #19579, #11183, #10335, #21440, #20869, #18096, #9547, #9370, #15129, #20001, #21463, #1568, #16823, #7893 ) ) ;
#17018 = TOROIDAL_SURFACE ( 'NONE', #12619, 4.000000000000000000, 2.000000000000000000 ) ;
#17019 = ORIENTED_EDGE ( 'NONE', *, *, #8641, .T. ) ;
#17020 = CARTESIAN_POINT ( 'NONE',  ( -51.88617280806869303, 111.6760431855662716, -46.69719173690569392 ) ) ;
#17021 = CARTESIAN_POINT ( 'NONE',  ( 14.55162269530302943, 189.3886954157946434, 320.5815939255251124 ) ) ;
#17022 = FACE_OUTER_BOUND ( 'NONE', #1522, .T. ) ;
#17023 = DIRECTION ( 'NONE',  ( 0.9999164797902015955, 0.000000000000000000, -0.01292414190464144692 ) ) ;
#17024 = CIRCLE ( 'NONE', #6388, 4.200000000000005507 ) ;
#17025 = DIRECTION ( 'NONE',  ( -0.01292394549866739996, -0.005513023399721131770, -0.9999012842304692006 ) ) ;
#17026 = VECTOR ( 'NONE', #21856, 1000.000000000000114 ) ;
#17027 = DIRECTION ( 'NONE',  ( -0.3102455404053335308, -0.9506564598521395348, 0.000000000000000000 ) ) ;
#17028 = ORIENTED_EDGE ( 'NONE', *, *, #12573, .T. ) ;
#17029 = VERTEX_POINT ( 'NONE', #12151 ) ;
#17030 = PLANE ( 'NONE',  #898 ) ;
#17031 = DIRECTION ( 'NONE',  ( 0.01292414190464117631, 5.551059884324760964E-17, 0.9999164797902015955 ) ) ;
#17032 = DIRECTION ( 'NONE',  ( -0.01292394549866733230, -0.005513023399720419666, -0.9999012842304692006 ) ) ;
#17033 = VERTEX_POINT ( 'NONE', #22231 ) ;
#17034 = CARTESIAN_POINT ( 'NONE',  ( 40.65822637310714782, 91.17157287525387233, 84.25167897319538213 ) ) ;
#17035 = TOROIDAL_SURFACE ( 'NONE', #4895, 0.01000000000000002623, 1.989999999999999991 ) ;
#17036 = AXIS2_PLACEMENT_3D ( 'NONE', #10563, #5261, #17583 ) ;
#17037 = ORIENTED_EDGE ( 'NONE', *, *, #3449, .F. ) ;
#17038 = CARTESIAN_POINT ( 'NONE',  ( 48.49194500006319686, 95.17841068403271265, -45.02347578433171549 ) ) ;
#17039 = EDGE_CURVE ( 'NONE', #18312, #9274, #14039, .T. ) ;
#17040 = CARTESIAN_POINT ( 'NONE',  ( -106.8724933792760652, 79.04398536104956463, -26.04362031086678897 ) ) ;
#17041 = EDGE_CURVE ( 'NONE', #6883, #10450, #3799, .T. ) ;
#17042 = ORIENTED_EDGE ( 'NONE', *, *, #9722, .F. ) ;
#17043 = VECTOR ( 'NONE', #19982, 1000.000000000000114 ) ;
#17044 = VECTOR ( 'NONE', #12948, 1000.000000000000000 ) ;
#17045 = CARTESIAN_POINT ( 'NONE',  ( -88.16567064151804800, 88.46953439568457611, 52.72066168997965718 ) ) ;
#17046 = ORIENTED_EDGE ( 'NONE', *, *, #19791, .T. ) ;
#17047 = B_SPLINE_CURVE_WITH_KNOTS ( 'NONE', 3,
 ( #10756, #299, #21303, #9245, #18120, #12602 ),
 .UNSPECIFIED., .F., .F.,
 ( 4, 2, 4 ),
 ( 2.380730969749054296E-07, 0.002629065763328481894, 0.005257893453559989508 ),
 .UNSPECIFIED. ) ;
#17048 = FACE_OUTER_BOUND ( 'NONE', #18411, .T. ) ;
#17049 = DIRECTION ( 'NONE',  ( 0.01292394549866739822, 0.005513023399721908059, 0.9999012842304692006 ) ) ;
#17050 = CARTESIAN_POINT ( 'NONE',  ( -25.07234391868265178, 89.37624705348630982, -78.14501733294019914 ) ) ;
#17051 = AXIS2_PLACEMENT_3D ( 'NONE', #17205, #19139, #12391 ) ;
#17052 = DIRECTION ( 'NONE',  ( 5.440186201345785633E-18, 1.000000000000000000, 1.334940939666367878E-17 ) ) ;
#17053 = LINE ( 'NONE', #8068, #11885 ) ;
#17054 = CARTESIAN_POINT ( 'NONE',  ( -51.96399215116387182, 189.4900423377766003, -91.89035338882484893 ) ) ;
#17055 = VERTEX_POINT ( 'NONE', #20860 ) ;
#17056 = ORIENTED_EDGE ( 'NONE', *, *, #10393, .F. ) ;
#17057 = FACE_OUTER_BOUND ( 'NONE', #1855, .T. ) ;
#17058 = DIRECTION ( 'NONE',  ( 0.01292394549866738608, 0.005513023399720699824, 0.9999012842304692006 ) ) ;
#17059 = LINE ( 'NONE', #8521, #13128 ) ;
#17060 = AXIS2_PLACEMENT_3D ( 'NONE', #2189, #4250, #16361 ) ;
#17061 = CARTESIAN_POINT ( 'NONE',  ( -52.23863840496477451, 118.9192529882356126, 167.5720208779842153 ) ) ;
#17062 = CIRCLE ( 'NONE', #13038, 9.000000000000005329 ) ;
#17063 = DIRECTION ( 'NONE',  ( 0.01111468050521496539, -0.5103046645782702839, 0.8599218645824316942 ) ) ;
#17064 = DIRECTION ( 'NONE',  ( 0.000000000000000000, 0.000000000000000000, 1.000000000000000000 ) ) ;
#17065 = DIRECTION ( 'NONE',  ( -0.01292394549866632963, -0.005513023399716958026, -0.9999012842304692006 ) ) ;
#17066 = CARTESIAN_POINT ( 'NONE',  ( -61.67972807482614428, 191.4143309225244707, 257.3032278304543183 ) ) ;
#17067 = VERTEX_POINT ( 'NONE', #4662 ) ;
#17068 = AXIS2_PLACEMENT_3D ( 'NONE', #2880, #6104, #13131 ) ;
#17069 = CARTESIAN_POINT ( 'NONE',  ( -12.83272386646220475, 184.4481542101678713, 276.9315297105506488 ) ) ;
#17070 = ORIENTED_EDGE ( 'NONE', *, *, #16983, .T. ) ;
#17071 = EDGE_CURVE ( 'NONE', #17630, #5976, #9622, .T. ) ;
#17072 = ORIENTED_EDGE ( 'NONE', *, *, #9799, .F. ) ;
#17073 = FACE_OUTER_BOUND ( 'NONE', #17509, .T. ) ;
#17074 = AXIS2_PLACEMENT_3D ( 'NONE', #16782, #20318, #20529 ) ;
#17075 = ORIENTED_EDGE ( 'NONE', *, *, #6294, .T. ) ;
#17076 = CARTESIAN_POINT ( 'NONE',  ( -51.07890516687701421, 106.8060942374655156, 71.59941146007480484 ) ) ;
#17077 = CARTESIAN_POINT ( 'NONE',  ( 0.000000000000000000, 18.00000000000000355, 0.000000000000000000 ) ) ;
#17078 = CARTESIAN_POINT ( 'NONE',  ( 105.4390993001727992, 77.44561610140188179, -31.34641640711175015 ) ) ;
#17079 = ADVANCED_FACE ( 'NONE', ( #20517 ), #18688, .T. ) ;
#17080 = DIRECTION ( 'NONE',  ( -0.9999164797902017066, -6.965998958219365988E-18, 0.01292414190464157356 ) ) ;
#17081 = VERTEX_POINT ( 'NONE', #9975 ) ;
#17082 = CARTESIAN_POINT ( 'NONE',  ( -13.36217923100928928, 326.0172268059896510, 372.0162718331554288 ) ) ;
#17083 = DIRECTION ( 'NONE',  ( -0.000000000000000000, -1.000000000000000000, -0.000000000000000000 ) ) ;
#17084 = VECTOR ( 'NONE', #1622, 1000.000000000000000 ) ;
#17085 = CARTESIAN_POINT ( 'NONE',  ( -79.92740525950245001, 54.99999999999999289, 6.133505399301367511 ) ) ;
#17086 = DIRECTION ( 'NONE',  ( 8.659560562354955045E-17, 0.7071067811865456854, -0.7071067811865493491 ) ) ;
#17087 = CARTESIAN_POINT ( 'NONE',  ( 2.067862704742617463, 72.00000000000000000, 159.9866367664322979 ) ) ;
#17088 = CARTESIAN_POINT ( 'NONE',  ( -36.81271860411143848, 93.81199595286604165, -82.30577144747519469 ) ) ;
#17089 = EDGE_LOOP ( 'NONE', ( #21926, #23, #4703, #22178 ) ) ;
#17090 = CARTESIAN_POINT ( 'NONE',  ( 86.24279638190517971, 74.99999999999998579, -1.114707239275309014 ) ) ;
#17091 = CARTESIAN_POINT ( 'NONE',  ( -8.468920434824459775, 185.4410853633842464, 308.0359439383103108 ) ) ;
#17092 = ORIENTED_EDGE ( 'NONE', *, *, #10853, .F. ) ;
#17093 = DIRECTION ( 'NONE',  ( -0.01292394549866740690, -0.005513023399721241925, -0.9999012842304693116 ) ) ;
#17094 = ADVANCED_FACE ( 'NONE', ( #3075 ), #10094, .T. ) ;
#17095 = ORIENTED_EDGE ( 'NONE', *, *, #2951, .T. ) ;
#17096 = ADVANCED_FACE ( 'NONE', ( #22336 ), #17905, .T. ) ;
#17097 = CARTESIAN_POINT ( 'NONE',  ( 15.07021670940958913, 186.4546686254222720, 322.6590458595396740 ) ) ;
#17098 = FACE_OUTER_BOUND ( 'NONE', #19576, .T. ) ;
#17099 = CYLINDRICAL_SURFACE ( 'NONE', #7290, 6.000000000000003553 ) ;
#17100 = EDGE_CURVE ( 'NONE', #10108, #19627, #549, .T. ) ;
#17101 = CARTESIAN_POINT ( 'NONE',  ( 19.58193934041550932, 146.5773600902072360, 276.3640708165659703 ) ) ;
#17102 = CARTESIAN_POINT ( 'NONE',  ( 14.16699832106635526, 189.6353986260119484, 320.6813409114420210 ) ) ;
#17103 = EDGE_CURVE ( 'NONE', #2719, #10523, #9261, .T. ) ;
#17104 = CARTESIAN_POINT ( 'NONE',  ( -64.99457118636308905, 169.9999999999999716, 0.8400692238016759239 ) ) ;
#17105 = CARTESIAN_POINT ( 'NONE',  ( 1.458023040593673859E-15, 2.000000000000000000, 9.999999999999994671 ) ) ;
#17106 = CARTESIAN_POINT ( 'NONE',  ( 70.91392079944854743, 72.00000000000000000, 84.09052168258639881 ) ) ;
#17107 = ORIENTED_EDGE ( 'NONE', *, *, #16695, .T. ) ;
#17108 = LINE ( 'NONE', #8678, #6295 ) ;
#17109 = DIRECTION ( 'NONE',  ( 1.490566292661454305E-14, 1.000000000000000000, -1.926591840573834312E-16 ) ) ;
#17110 = CARTESIAN_POINT ( 'NONE',  ( 153.9999999999992610, 0.000000000000000000, 53.76161406891468175 ) ) ;
#17111 = DIRECTION ( 'NONE',  ( 0.01292394549866733230, 0.005513023399720419666, 0.9999012842304692006 ) ) ;
#17112 = MANIFOLD_SOLID_BREP ( 'Stock-MAS-425-1', #16277 ) ;
#17113 = LINE ( 'NONE', #4910, #15783 ) ;
#17114 = ADVANCED_FACE ( 'NONE', ( #5349 ), #14569, .F. ) ;
#17115 = CARTESIAN_POINT ( 'NONE',  ( -5.672696058028122934, 70.55846734465492887, -98.91173476717540325 ) ) ;
#17116 = CARTESIAN_POINT ( 'NONE',  ( 58.13167081004702652, 143.2710928180444796, 48.49959442800333420 ) ) ;
#17117 = CARTESIAN_POINT ( 'NONE',  ( -10.85595612533484911, 109.6999345499266525, 127.2773526115149281 ) ) ;
#17118 = ORIENTED_EDGE ( 'NONE', *, *, #2341, .F. ) ;
#17119 = DIRECTION ( 'NONE',  ( 7.125109674161246868E-05, -0.9999848031710253382, 0.005512562950850155054 ) ) ;
#17120 = ORIENTED_EDGE ( 'NONE', *, *, #22408, .T. ) ;
#17121 = DIRECTION ( 'NONE',  ( -0.000000000000000000, -1.000000000000000000, -0.000000000000000000 ) ) ;
#17122 = DIRECTION ( 'NONE',  ( -0.01292394549866738782, -0.005513023399720700692, -0.9999012842304693116 ) ) ;
#17123 = ORIENTED_EDGE ( 'NONE', *, *, #8750, .T. ) ;
#17124 = CARTESIAN_POINT ( 'NONE',  ( -41.61793149762837629, 69.99999999999998579, -86.46934588545651934 ) ) ;
#17125 = VERTEX_POINT ( 'NONE', #21530 ) ;
#17126 = EDGE_CURVE ( 'NONE', #14478, #3464, #16521, .T. ) ;
#17127 = CARTESIAN_POINT ( 'NONE',  ( 49.43718378874159214, 109.1839087875310810, -47.09652170433833618 ) ) ;
#17128 = ORIENTED_EDGE ( 'NONE', *, *, #2712, .T. ) ;
#17129 = LINE ( 'NONE', #6549, #416 ) ;
#17130 = DIRECTION ( 'NONE',  ( 7.125109674161246868E-05, -0.9999848031710253382, 0.005512562950850155054 ) ) ;
#17131 = CARTESIAN_POINT ( 'NONE',  ( 1.163172771417732010, 45.00000000000000000, 89.99248318111813205 ) ) ;
#17132 = DIRECTION ( 'NONE',  ( -0.01096700916508639573, 0.5290868411612598132, -0.8484968115555726609 ) ) ;
#17133 = FACE_OUTER_BOUND ( 'NONE', #21354, .T. ) ;
#17134 = DIRECTION ( 'NONE',  ( -0.9999164797902015955, -2.001050586450176109E-22, 0.01292414190464270113 ) ) ;
#17135 = ORIENTED_EDGE ( 'NONE', *, *, #15583, .F. ) ;
#17136 = EDGE_CURVE ( 'NONE', #8712, #8420, #14688, .T. ) ;
#17137 = CARTESIAN_POINT ( 'NONE',  ( 47.98905872121961380, 95.04270968059627478, -44.78735749829896662 ) ) ;
#17138 = ADVANCED_FACE ( 'NONE', ( #4422, #11114, #2724 ), #18135, .F. ) ;
#17139 = CARTESIAN_POINT ( 'NONE',  ( 41.42670316190684332, 94.99786382055523859, -44.62631324292065926 ) ) ;
#17140 = ORIENTED_EDGE ( 'NONE', *, *, #9222, .F. ) ;
#17141 = CARTESIAN_POINT ( 'NONE',  ( -41.00000899811524846, 169.5540992312279229, 273.1580453575298293 ) ) ;
#17142 = CARTESIAN_POINT ( 'NONE',  ( -90.13126742504640276, 87.37348474049055369, 51.17112193263445619 ) ) ;
#17143 = ORIENTED_EDGE ( 'NONE', *, *, #5603, .F. ) ;
#17144 = DIRECTION ( 'NONE',  ( 0.1296504907605110779, 0.005475273188902231650, 0.9915446392518419971 ) ) ;
#17145 = LINE ( 'NONE', #8509, #18065 ) ;
#17146 = CARTESIAN_POINT ( 'NONE',  ( -2.523753925720915614, 86.15700740604867747, -74.98433394420648312 ) ) ;
#17147 = CARTESIAN_POINT ( 'NONE',  ( 49.46148465141350670, 112.8301064087732897, -44.82848384907012473 ) ) ;
#17148 = CIRCLE ( 'NONE', #19335, 7.921742784567035400 ) ;
#17149 = CARTESIAN_POINT ( 'NONE',  ( -53.19734013806819206, 189.4876967392748384, -92.29990616481009624 ) ) ;
#17150 = EDGE_LOOP ( 'NONE', ( #12543, #11998, #5478, #13770, #8611, #6059 ) ) ;
#17151 = EDGE_CURVE ( 'NONE', #10015, #11275, #16752, .T. ) ;
#17152 = EDGE_LOOP ( 'NONE', ( #8328, #5462, #18117, #13634 ) ) ;
#17153 = ADVANCED_FACE ( 'NONE', ( #16412 ), #21640, .F. ) ;
#17154 = LINE ( 'NONE', #7958, #19442 ) ;
#17155 = CARTESIAN_POINT ( 'NONE',  ( -42.56982644846065966, 144.7550503794368524, -43.81497911448970228 ) ) ;
#17156 = CARTESIAN_POINT ( 'NONE',  ( 90.43417961988760112, 79.20545292891344502, -29.12427242046056008 ) ) ;
#17157 = DIRECTION ( 'NONE',  ( -0.01035358732338034077, 0.000000000000000000, -0.9999464001782980560 ) ) ;
#17158 = CARTESIAN_POINT ( 'NONE',  ( -12.56198361051020918, 146.5221865386392324, 276.8288772454161517 ) ) ;
#17159 = VERTEX_POINT ( 'NONE', #7771 ) ;
#17160 = SHAPE_REPRESENTATION_RELATIONSHIP ( 'NONE' , 'NONE' ,  #5468, #7450 ) ;
#17161 = CARTESIAN_POINT ( 'NONE',  ( -5.365183637746670620, 172.6234054757072727, 299.6832001106340613 ) ) ;
#17162 = DIRECTION ( 'NONE',  ( 0.01292394549866738782, 0.005513023399720700692, 0.9999012842304693116 ) ) ;
#17163 = VERTEX_POINT ( 'NONE', #6472 ) ;
#17164 = ORIENTED_EDGE ( 'NONE', *, *, #396, .F. ) ;
#17165 = AXIS2_PLACEMENT_3D ( 'NONE', #17131, #15203, #13467 ) ;
#17166 = CARTESIAN_POINT ( 'NONE',  ( 50.84062004008612234, 101.1708071963161615, 64.71406976224261598 ) ) ;
#17167 = AXIS2_PLACEMENT_3D ( 'NONE', #3310, #20769, #8364 ) ;
#17169 = EDGE_LOOP ( 'NONE', ( #22585, #16733, #21899, #7847 ) ) ;
#17168 = ORIENTED_EDGE ( 'NONE', *, *, #21404, .T. ) ;
#17170 = CARTESIAN_POINT ( 'NONE',  ( -65.56567718511387000, 113.4816418249608034, -43.34532459741677002 ) ) ;
#17171 = DIRECTION ( 'NONE',  ( 0.01292394549866738782, 0.005513023399721118760, 0.9999012842304692006 ) ) ;
#17172 = CIRCLE ( 'NONE', #22271, 2.000000000000001776 ) ;
#17173 = DIRECTION ( 'NONE',  ( 0.000000000000000000, 1.000000000000000000, -0.000000000000000000 ) ) ;
#17174 = CARTESIAN_POINT ( 'NONE',  ( -93.17671387018313567, 79.04398536104955042, -26.22064129356660800 ) ) ;
#17175 = DIRECTION ( 'NONE',  ( 0.9999164797902017066, 6.965998958219367529E-18, -0.01292414190464157182 ) ) ;
#17176 = FACE_OUTER_BOUND ( 'NONE', #19738, .T. ) ;
#17177 = VERTEX_POINT ( 'NONE', #22179 ) ;
#17178 = CARTESIAN_POINT ( 'NONE',  ( 41.09169241204631362, 95.99012513974443550, 84.20368898025243709 ) ) ;
#17179 = FACE_OUTER_BOUND ( 'NONE', #4452, .T. ) ;
#17180 = CARTESIAN_POINT ( 'NONE',  ( -51.04847592823571034, 189.5933835232740989, -73.15598528727107919 ) ) ;
#17181 = VECTOR ( 'NONE', #2516, 1000.000000000000114 ) ;
#17182 = APPLICATION_CONTEXT ( 'automotive_design' ) ;
#17183 = DIRECTION ( 'NONE',  ( -0.000000000000000000, -1.000000000000000000, -0.000000000000000000 ) ) ;
#17184 = ORIENTED_EDGE ( 'NONE', *, *, #4177, .F. ) ;
#17185 = DIRECTION ( 'NONE',  ( 0.9999164797902017066, 2.001050586450178931E-22, -0.01292414190464131508 ) ) ;
#17186 = FACE_OUTER_BOUND ( 'NONE', #17475, .T. ) ;
#17187 = VERTEX_POINT ( 'NONE', #3954 ) ;
#17188 = LINE ( 'NONE', #11922, #3949 ) ;
#17189 = TOROIDAL_SURFACE ( 'NONE', #12800, 124.0000000000000000, 2.000000000000000000 ) ;
#17190 = VERTEX_POINT ( 'NONE', #18125 ) ;
#17191 = CARTESIAN_POINT ( 'NONE',  ( -70.91392079944854743, 72.00000000000000000, -84.09052168258642723 ) ) ;
#17192 = VERTEX_POINT ( 'NONE', #11751 ) ;
#17193 = CARTESIAN_POINT ( 'NONE',  ( -38.21549050681395698, 167.4026153394593734, 273.1339171915171846 ) ) ;
#17194 = CARTESIAN_POINT ( 'NONE',  ( -63.91983116576977153, 91.51644034066822542, 67.07156771589210109 ) ) ;
#17195 = ORIENTED_EDGE ( 'NONE', *, *, #18352, .F. ) ;
#17196 = CARTESIAN_POINT ( 'NONE',  ( 15.34006562386835881, 188.8538180965162780, 320.3317479991936239 ) ) ;
#17197 = ORIENTED_EDGE ( 'NONE', *, *, #7817, .F. ) ;
#17198 = VECTOR ( 'NONE', #9414, 1000.000000000000000 ) ;
#17199 = EDGE_CURVE ( 'NONE', #7316, #7202, #22438, .T. ) ;
#17200 = EDGE_CURVE ( 'NONE', #4784, #9640, #13484, .T. ) ;
#17201 = FACE_OUTER_BOUND ( 'NONE', #21555, .T. ) ;
#17202 = CYLINDRICAL_SURFACE ( 'NONE', #2281, 110.5324305509042233 ) ;
#17203 = EDGE_CURVE ( 'NONE', #2844, #22542, #16628, .T. ) ;
#17204 = AXIS2_PLACEMENT_3D ( 'NONE', #3931, #16269, #736 ) ;
#17205 = CARTESIAN_POINT ( 'NONE',  ( 13.80509744631564750, 155.5569384583423300, 100.8921482990249956 ) ) ;
#17206 = ORIENTED_EDGE ( 'NONE', *, *, #8656, .T. ) ;
#17207 = DIRECTION ( 'NONE',  ( -5.440186201345785633E-18, -1.000000000000000000, -1.334940939666367878E-17 ) ) ;
#17208 = CARTESIAN_POINT ( 'NONE',  ( 64.99770623461974139, 126.0006686604749291, -0.5975164539643176287 ) ) ;
#17209 = FACE_OUTER_BOUND ( 'NONE', #18219, .T. ) ;
#17210 = FACE_OUTER_BOUND ( 'NONE', #6262, .T. ) ;
#17211 = ADVANCED_FACE ( 'NONE', ( #4074 ), #20459, .F. ) ;
#17212 = CARTESIAN_POINT ( 'NONE',  ( 9.143211457558962252, 165.4878736975560969, 88.39641525520653431 ) ) ;
#17213 = ADVANCED_FACE ( 'NONE', ( #7418 ), #9804, .F. ) ;
#17214 = CIRCLE ( 'NONE', #5838, 9.999999999999998224 ) ;
#17215 = FACE_OUTER_BOUND ( 'NONE', #4253, .T. ) ;
#17216 = CARTESIAN_POINT ( 'NONE',  ( -109.6289368035922536, 77.12912189496637438, 29.41931704363613420 ) ) ;
#17217 = ADVANCED_FACE ( 'NONE', ( #20238 ), #1924, .T. ) ;
#17218 = CONTEXT_DEPENDENT_SHAPE_REPRESENTATION ( #11182, #11957 ) ;
#17219 = AXIS2_PLACEMENT_3D ( 'NONE', #11702, #13545, #18695 ) ;
#17220 = VERTEX_POINT ( 'NONE', #21521 ) ;
#17221 = DIRECTION ( 'NONE',  ( -0.01292394549866772609, -0.005513023399720218438, -0.9999012842304693116 ) ) ;
#17222 = FACE_OUTER_BOUND ( 'NONE', #16961, .T. ) ;
#17223 = LINE ( 'NONE', #1286, #7394 ) ;
#17224 = DIRECTION ( 'NONE',  ( 0.01292394549866738608, 0.005513023399720699824, 0.9999012842304692006 ) ) ;
#17225 = VERTEX_POINT ( 'NONE', #9249 ) ;
#17226 = EDGE_CURVE ( 'NONE', #984, #17835, #4836, .T. ) ;
#17227 = EDGE_LOOP ( 'NONE', ( #11553, #15795, #18230 ) ) ;
#17228 = CARTESIAN_POINT ( 'NONE',  ( -4.356009107694418958, 172.5947582827599831, 324.3400096493597289 ) ) ;
#17229 = DIRECTION ( 'NONE',  ( 0.01292394549866740169, 0.005513023399721131770, 0.9999012842304693116 ) ) ;
#17230 = ORIENTED_EDGE ( 'NONE', *, *, #1363, .F. ) ;
#17231 = ADVANCED_FACE ( 'NONE', ( #1073 ), #1198, .F. ) ;
#17232 = CARTESIAN_POINT ( 'NONE',  ( 49.61333693951482360, 109.9750644004051594, -47.38601841831088990 ) ) ;
#17233 = ORIENTED_EDGE ( 'NONE', *, *, #19718, .F. ) ;
#17234 = DIRECTION ( 'NONE',  ( 0.000000000000000000, 0.000000000000000000, 1.000000000000000000 ) ) ;
#17235 = EDGE_CURVE ( 'NONE', #19636, #956, #20622, .T. ) ;
#17236 = DIRECTION ( 'NONE',  ( -0.9999164797902015955, -6.965998958219364448E-18, 0.01292414190464157182 ) ) ;
#17237 = DIRECTION ( 'NONE',  ( -0.9999164797902015955, -6.965998958219364448E-18, 0.01292414190464157182 ) ) ;
#17238 = PLANE ( 'NONE',  #15128 ) ;
#17239 = AXIS2_PLACEMENT_3D ( 'NONE', #2062, #7225, #17706 ) ;
#17240 = ADVANCED_FACE ( 'NONE', ( #20357 ), #11836, .T. ) ;
#17241 = AXIS2_PLACEMENT_3D ( 'NONE', #20915, #4831, #5290 ) ;
#17242 = PLANE ( 'NONE',  #12979 ) ;
#17243 = LINE ( 'NONE', #8608, #9748 ) ;
#17244 = VECTOR ( 'NONE', #3180, 1000.000000000000000 ) ;
#17245 = ORIENTED_EDGE ( 'NONE', *, *, #9701, .T. ) ;
#17246 = CARTESIAN_POINT ( 'NONE',  ( -41.48139093415068146, 161.8450704598839138, 269.2063766754258722 ) ) ;
#17247 = CIRCLE ( 'NONE', #18354, 1.999999999999998224 ) ;
#17248 = DIRECTION ( 'NONE',  ( 7.125109674161246868E-05, -0.9999848031710252272, 0.005512562950850154186 ) ) ;
#17249 = ORIENTED_EDGE ( 'NONE', *, *, #20579, .T. ) ;
#17250 = CARTESIAN_POINT ( 'NONE',  ( -8.312614011469616315, 81.99999999999998579, -95.45924547291811280 ) ) ;
#17251 = CARTESIAN_POINT ( 'NONE',  ( -90.05921627452258349, 88.59350953919012284, 52.64378069695336393 ) ) ;
#17252 = EDGE_CURVE ( 'NONE', #11923, #1810, #8065, .T. ) ;
#17253 = AXIS2_PLACEMENT_3D ( 'NONE', #5925, #12963, #9737 ) ;
#17254 = ORIENTED_EDGE ( 'NONE', *, *, #15886, .F. ) ;
#17255 = AXIS2_PLACEMENT_3D ( 'NONE', #3018, #4840, #11877 ) ;
#17256 = ORIENTED_EDGE ( 'NONE', *, *, #11170, .F. ) ;
#17257 = CARTESIAN_POINT ( 'NONE',  ( -9.955606456259319614, 184.2243514862264533, 323.1466302186144617 ) ) ;
#17258 = DIRECTION ( 'NONE',  ( 0.01292394549866695240, 0.005513023399725255208, 0.9999012842304693116 ) ) ;
#17259 = CARTESIAN_POINT ( 'NONE',  ( 88.82263333796723259, 169.9999999999999716, -1.148052203164690033 ) ) ;
#17260 = CARTESIAN_POINT ( 'NONE',  ( -5.871648968083818865, 81.99999999999998579, -88.03282711297042340 ) ) ;
#17261 = CARTESIAN_POINT ( 'NONE',  ( 81.08638132281690503, 75.13007332810629180, -6.018189424661123610 ) ) ;
#17262 = AXIS2_PLACEMENT_3D ( 'NONE', #20942, #19337, #8748 ) ;
#17263 = CYLINDRICAL_SURFACE ( 'NONE', #20305, 2.499999999999988010 ) ;
#17264 = EDGE_LOOP ( 'NONE', ( #5149, #9536 ) ) ;
#17265 = EDGE_CURVE ( 'NONE', #10504, #2665, #14677, .T. ) ;
#17266 = CIRCLE ( 'NONE', #6240, 10.00000000000001421 ) ;
#17267 = EDGE_LOOP ( 'NONE', ( #15504, #13252, #19612, #1257 ) ) ;
#17268 = EDGE_LOOP ( 'NONE', ( #17549, #15465, #18252, #11896 ) ) ;
#17269 = FACE_OUTER_BOUND ( 'NONE', #11687, .T. ) ;
#17270 = CARTESIAN_POINT ( 'NONE',  ( 8.996640567037356817, 190.2633029501699014, 274.5811317046487829 ) ) ;
#17271 = CARTESIAN_POINT ( 'NONE',  ( 17.00040199784601214, 187.3380220790077431, 319.4296498798100288 ) ) ;
#17272 = CARTESIAN_POINT ( 'NONE',  ( -40.94471193931616426, 95.70788552361970858, 82.69081069369302384 ) ) ;
#17273 = CARTESIAN_POINT ( 'NONE',  ( -6.941700055406210268, 144.5720018159295819, 276.5112050013826206 ) ) ;
#17274 =( LENGTH_UNIT ( ) NAMED_UNIT ( * ) SI_UNIT ( .MILLI., .METRE. ) );
#17275 = DIRECTION ( 'NONE',  ( -0.5089394657577703818, -0.004781488884709769391, -0.8607890319690654213 ) ) ;
#17276 = AXIS2_PLACEMENT_3D ( 'NONE', #4846, #3363, #8408 ) ;
#17277 = PRODUCT_DEFINITION_SHAPE ( 'NONE', 'NONE',  #22696 ) ;
#17278 = VECTOR ( 'NONE', #1574, 999.9999999999998863 ) ;
#17279 = VECTOR ( 'NONE', #16963, 1000.000000000000000 ) ;
#17280 = CARTESIAN_POINT ( 'NONE',  ( 12.73831384893346197, 160.9807657804660153, 324.1830962737362256 ) ) ;
#17281 = ORIENTED_EDGE ( 'NONE', *, *, #3771, .T. ) ;
#17282 = ORIENTED_EDGE ( 'NONE', *, *, #532, .T. ) ;
#17283 = VERTEX_POINT ( 'NONE', #15226 ) ;
#17284 = DIRECTION ( 'NONE',  ( -0.01292394549866740343, -0.005513023399721215904, -0.9999012842304693116 ) ) ;
#17285 = EDGE_CURVE ( 'NONE', #552, #6085, #6236, .T. ) ;
#17286 = AXIS2_PLACEMENT_3D ( 'NONE', #18465, #20159, #1123 ) ;
#17287 = EDGE_CURVE ( 'NONE', #9119, #9213, #12576, .T. ) ;
#17289 = ORIENTED_EDGE ( 'NONE', *, *, #21417, .T. ) ;
#17288 = VERTEX_POINT ( 'NONE', #8195 ) ;
#17290 = CARTESIAN_POINT ( 'NONE',  ( -1.089749515181836320E-13, 20.00000000000000000, 7.999999999999994671 ) ) ;
#17291 = CARTESIAN_POINT ( 'NONE',  ( -88.09114847236423884, 72.29207065074294292, 61.95466991546196311 ) ) ;
#17292 = B_SPLINE_CURVE_WITH_KNOTS ( 'NONE', 3,
 ( #22308, #22089, #15474, #1109 ),
 .UNSPECIFIED., .F., .F.,
 ( 4, 4 ),
 ( 0.000000000000000000, 0.0001181342984831720616 ),
 .UNSPECIFIED. ) ;
#17293 = CARTESIAN_POINT ( 'NONE',  ( -64.99457118636311748, 170.0000000000008242, 0.8400692238025471159 ) ) ;
#17294 = VECTOR ( 'NONE', #16053, 1000.000000000000000 ) ;
#17295 = FACE_OUTER_BOUND ( 'NONE', #5994, .T. ) ;
#17296 = CARTESIAN_POINT ( 'NONE',  ( 66.18268079339601684, 69.99999999999998579, -87.86269266872859873 ) ) ;
#17297 = CARTESIAN_POINT ( 'NONE',  ( 42.19468217728159942, 94.63733313072589226, 82.98836926700062122 ) ) ;
#17298 = DIRECTION ( 'NONE',  ( -0.9999164797902017066, 0.000000000000000000, 0.01292414190464157529 ) ) ;
#17299 = VECTOR ( 'NONE', #16827, 1000.000000000000114 ) ;
#17300 = CARTESIAN_POINT ( 'NONE',  ( 11.72327481064200683, 187.7930371575377535, 304.8675929460329144 ) ) ;
#17301 = CYLINDRICAL_SURFACE ( 'NONE', #17802, 3.399999999999991918 ) ;
#17302 = DIRECTION ( 'NONE',  ( 2.025474946048326158E-22, -1.000000000000000000, 1.876735158486679638E-22 ) ) ;
#17303 = VECTOR ( 'NONE', #2358, 1000.000000000000114 ) ;
#17304 = DIRECTION ( 'NONE',  ( -0.6979091139780387865, 0.003898296230782336263, 0.7161757269782926816 ) ) ;
#17305 = PLANE ( 'NONE',  #17661 ) ;
#17306 = ORIENTED_EDGE ( 'NONE', *, *, #14129, .F. ) ;
#17307 = CARTESIAN_POINT ( 'NONE',  ( 1.163172771417732010, 69.99999999999998579, 89.99248318111813205 ) ) ;
#17308 = ORIENTED_EDGE ( 'NONE', *, *, #1657, .T. ) ;
#17309 = AXIS2_PLACEMENT_3D ( 'NONE', #19438, #10600, #21266 ) ;
#17310 = EDGE_CURVE ( 'NONE', #5640, #15200, #21602, .T. ) ;
#17311 = AXIS2_PLACEMENT_3D ( 'NONE', #19046, #9997, #20662 ) ;
#17312 = DIRECTION ( 'NONE',  ( 0.01292394549866733404, 0.005513023399720420534, 0.9999012842304693116 ) ) ;
#17313 = VECTOR ( 'NONE', #21320, 999.9999999999998863 ) ;
#17314 = ORIENTED_EDGE ( 'NONE', *, *, #16284, .F. ) ;
#17315 = FACE_OUTER_BOUND ( 'NONE', #15985, .T. ) ;
#17316 = SURFACE_STYLE_FILL_AREA ( #20967 ) ;
#17317 = DIRECTION ( 'NONE',  ( 0.000000000000000000, 0.000000000000000000, 1.000000000000000000 ) ) ;
#17318 = B_SPLINE_CURVE_WITH_KNOTS ( 'NONE', 3,
 ( #328, #7319, #908, #7444, #21770, #16207, #4213, #7658, #19708, #3977, #9154, #11241, #11001, #674, #14936, #9633, #7898, #5942 ),
 .UNSPECIFIED., .F., .F.,
 ( 4, 2, 2, 2, 2, 2, 2, 2, 4 ),
 ( -3.889482208294626299E-05, 0.0005389813427436562733, 0.001116857507570258789, 0.001694733672396861197, 0.002272609837223463821, 0.002850486002050066445, 0.003428362166876668636, 0.004006238331703271260, 0.004584114496529873885 ),
 .UNSPECIFIED. ) ;
#17319 = ORIENTED_EDGE ( 'NONE', *, *, #16760, .T. ) ;
#17320 = PLANE ( 'NONE',  #4715 ) ;
#17321 = ORIENTED_EDGE ( 'NONE', *, *, #4440, .T. ) ;
#17322 = CIRCLE ( 'NONE', #20600, 78.99999999999998579 ) ;
#17323 = CARTESIAN_POINT ( 'NONE',  ( 64.31884524158141403, 144.7109461922390778, -53.19708549627201677 ) ) ;
#17324 = AXIS2_PLACEMENT_3D ( 'NONE', #17919, #2154, #11128 ) ;
#17325 = AXIS2_PLACEMENT_3D ( 'NONE', #16878, #6305, #20069 ) ;
#17326 = PRODUCT_RELATED_PRODUCT_CATEGORY ( 'part', '', ( #5355 ) ) ;
#17327 = CARTESIAN_POINT ( 'NONE',  ( -65.90110554552374822, 105.0000000000000000, -69.29678410920486442 ) ) ;
#17328 =( LENGTH_UNIT ( ) NAMED_UNIT ( * ) SI_UNIT ( .MILLI., .METRE. ) );
#17329 = CARTESIAN_POINT ( 'NONE',  ( 13.42006642051110177, 160.8124487847600221, 323.5078865155649055 ) ) ;
#17330 = ORIENTED_EDGE ( 'NONE', *, *, #29, .T. ) ;
#17331 = CARTESIAN_POINT ( 'NONE',  ( 38.69757710431291287, 94.02752048664899576, 82.47923521851859618 ) ) ;
#17332 = CARTESIAN_POINT ( 'NONE',  ( -92.43457499998879712, 77.12912189496637438, 31.19724316448926160 ) ) ;
#17333 = AXIS2_PLACEMENT_3D ( 'NONE', #6682, #1416, #22499 ) ;
#17334 = DIRECTION ( 'NONE',  ( 0.01292394549866738782, 0.005513023399720468239, 0.9999012842304692006 ) ) ;
#17335 = MANIFOLD_SOLID_BREP ( 'Stock-MAS-425-1', #3262 ) ;
#17336 = ORIENTED_EDGE ( 'NONE', *, *, #9407, .F. ) ;
#17337 = CARTESIAN_POINT ( 'NONE',  ( 20.60016704620528571, 181.9681718854236294, 313.0792466296721841 ) ) ;
#17338 = CYLINDRICAL_SURFACE ( 'NONE', #5280, 3.099999999999998757 ) ;
#17339 = EDGE_LOOP ( 'NONE', ( #21269, #17484 ) ) ;
#17340 = CIRCLE ( 'NONE', #465, 78.99999999999998579 ) ;
#17341 = EDGE_CURVE ( 'NONE', #17190, #18283, #15779, .T. ) ;
#17342 = CYLINDRICAL_SURFACE ( 'NONE', #2903, 2.000000000000008438 ) ;
#17343 = FACE_OUTER_BOUND ( 'NONE', #1036, .T. ) ;
#17344 = ITEM_DEFINED_TRANSFORMATION ( 'NONE', 'NONE', #18723,  #6292 ) ;
#17345 = DIRECTION ( 'NONE',  ( 0.9999164797902015955, 6.965998958219364448E-18, -0.01292414190464157182 ) ) ;
#17346 = VERTEX_POINT ( 'NONE', #7024 ) ;
#17347 = FACE_OUTER_BOUND ( 'NONE', #10244, .T. ) ;
#17348 = CARTESIAN_POINT ( 'NONE',  ( 10.89474438599883221, 174.2127514147958891, 324.4667421121108646 ) ) ;
#17349 = DIRECTION ( 'NONE',  ( -0.01292394549866727679, -0.005513023399720743192, -0.9999012842304693116 ) ) ;
#17350 = CIRCLE ( 'NONE', #7436, 2.000000000000001776 ) ;
#17351 = DIRECTION ( 'NONE',  ( 7.125109674160325297E-05, -0.9999848031710252272, 0.005512562950849327591 ) ) ;
#17352 = EDGE_LOOP ( 'NONE', ( #20056, #3210, #2444 ) ) ;
#17353 = CARTESIAN_POINT ( 'NONE',  ( 21.71998689217155132, 185.4674263880815204, 276.2600312189053966 ) ) ;
#17354 = DIRECTION ( 'NONE',  ( 7.125109674364534776E-05, -0.9999848031710252272, 0.005512562950849704893 ) ) ;
#17355 = EDGE_CURVE ( 'NONE', #5608, #10157, #13923, .T. ) ;
#17356 = ORIENTED_EDGE ( 'NONE', *, *, #7603, .F. ) ;
#17357 = CARTESIAN_POINT ( 'NONE',  ( -12.58378492319879705, 109.7167104967248434, 130.3428598364639299 ) ) ;
#17358 = ORIENTED_EDGE ( 'NONE', *, *, #15094, .T. ) ;
#17359 = CARTESIAN_POINT ( 'NONE',  ( 106.8724933792760226, 79.04398536104964990, 26.04362031086705542 ) ) ;
#17360 = DIRECTION ( 'NONE',  ( 0.9934404589540163366, 0.1135548637187057813, -0.01346653032742924430 ) ) ;
#17361 = LINE ( 'NONE', #2068, #814 ) ;
#17362 = VECTOR ( 'NONE', #12514, 1000.000000000000000 ) ;
#17363 = EDGE_CURVE ( 'NONE', #9319, #7137, #20149, .T. ) ;
#17364 = DIRECTION ( 'NONE',  ( -0.01292394549866750231, -0.005513023399722823126, -0.9999012842304692006 ) ) ;
#17365 = DIRECTION ( 'NONE',  ( -0.000000000000000000, -1.000000000000000000, -0.000000000000000000 ) ) ;
#17366 = ORIENTED_EDGE ( 'NONE', *, *, #2625, .T. ) ;
#17367 = CARTESIAN_POINT ( 'NONE',  ( -0.003538370294055813436, 81.99999999999998579, -98.91746206376724615 ) ) ;
#17368 = VERTEX_POINT ( 'NONE', #15776 ) ;
#17369 = EDGE_CURVE ( 'NONE', #10824, #2768, #16165, .T. ) ;
#17370 = DIRECTION ( 'NONE',  ( 2.025474946048326158E-22, -1.000000000000000000, 1.876735158486679638E-22 ) ) ;
#17371 = CARTESIAN_POINT ( 'NONE',  ( -90.15853200097006948, 87.23282554233360031, 51.25677079265641112 ) ) ;
#17372 = EDGE_CURVE ( 'NONE', #21806, #4475, #6572, .T. ) ;
#17373 = SHAPE_REPRESENTATION ( 'Holder', ( #6292 ), #10694 ) ;
#17374 = CARTESIAN_POINT ( 'NONE',  ( 1.117803423002105445, 55.00000000000000000, 109.6947150755565161 ) ) ;
#17375 = TOROIDAL_SURFACE ( 'NONE', #21030, 9.921742784567035400, 2.000000000000000000 ) ;
#17376 = MANIFOLD_SOLID_BREP ( 'Stock-MAS-425-1', #13198 ) ;
#17378 = EDGE_LOOP ( 'NONE', ( #7118, #12653, #21322, #5028 ) ) ;
#17377 = EDGE_LOOP ( 'NONE', ( #4210, #22575, #14022, #7981 ) ) ;
#17379 = CIRCLE ( 'NONE', #136, 1.999999999999999778 ) ;
#17380 = ORIENTED_EDGE ( 'NONE', *, *, #17685, .F. ) ;
#17381 = CARTESIAN_POINT ( 'NONE',  ( -8.663423201070779456, 185.1548080327998207, 323.2462545196998462 ) ) ;
#17382 = CARTESIAN_POINT ( 'NONE',  ( 43.19621557115664245, 121.2962013336460956, 247.0266759469006672 ) ) ;
#17383 = LINE ( 'NONE', #1638, #15009 ) ;
#17384 = CARTESIAN_POINT ( 'NONE',  ( -90.00000000000000000, 0.000000000000000000, 8.394090934816448357E-16 ) ) ;
#17385 = FACE_OUTER_BOUND ( 'NONE', #14354, .T. ) ;
#17386 = CARTESIAN_POINT ( 'NONE',  ( 19.42556530730579567, 136.7551719540686008, -44.57217540897067920 ) ) ;
#17387 = EDGE_CURVE ( 'NONE', #3348, #9064, #18332, .T. ) ;
#17388 = ORIENTED_EDGE ( 'NONE', *, *, #5044, .T. ) ;
#17389 = ORIENTED_EDGE ( 'NONE', *, *, #7971, .T. ) ;
#17390 = CARTESIAN_POINT ( 'NONE',  ( -9.975585911415770113, 186.6480926472742112, 277.9354835072872447 ) ) ;
#17391 = DIRECTION ( 'NONE',  ( -7.125109674161231961E-05, 0.9999848031710252272, -0.005512562950850142043 ) ) ;
#17392 = CIRCLE ( 'NONE', #8555, 26.23296215977917356 ) ;
#17393 = CARTESIAN_POINT ( 'NONE',  ( 17.14877061339265651, 185.1529327208830580, 321.7930803067964689 ) ) ;
#17394 = CARTESIAN_POINT ( 'NONE',  ( -90.01466456474447853, 70.04421420112709029, 63.22468240810439966 ) ) ;
#17395 = CARTESIAN_POINT ( 'NONE',  ( -65.56655171279719241, 125.7553391191873544, -43.41298515461679131 ) ) ;
#17396 = EDGE_CURVE ( 'NONE', #14225, #11656, #3645, .T. ) ;
#17397 = EDGE_LOOP ( 'NONE', ( #5758, #19430, #732 ) ) ;
#17398 = DIRECTION ( 'NONE',  ( 0.000000000000000000, 0.000000000000000000, 1.000000000000000000 ) ) ;
#17399 = PLANE ( 'NONE',  #19608 ) ;
#17400 = VECTOR ( 'NONE', #15666, 999.9999999999998863 ) ;
#17401 = CARTESIAN_POINT ( 'NONE',  ( 105.3709006619169912, 71.09718787230102066, -31.57492962159256322 ) ) ;
#17402 = VECTOR ( 'NONE', #17345, 1000.000000000000000 ) ;
#17403 = CARTESIAN_POINT ( 'NONE',  ( -105.6473595942261028, 69.99999999999998579, -30.63715735456343126 ) ) ;
#17404 = ORIENTED_EDGE ( 'NONE', *, *, #1139, .F. ) ;
#17405 = ORIENTED_EDGE ( 'NONE', *, *, #21105, .F. ) ;
#17406 = ORIENTED_EDGE ( 'NONE', *, *, #12907, .T. ) ;
#17407 = ADVANCED_FACE ( 'NONE', ( #8724 ), #12112, .F. ) ;
#17408 = AXIS2_PLACEMENT_3D ( 'NONE', #20781, #14255, #6773 ) ;
#17410 = ORIENTED_EDGE ( 'NONE', *, *, #6977, .T. ) ;
#17409 = ORIENTED_EDGE ( 'NONE', *, *, #7532, .F. ) ;
#17411 = CARTESIAN_POINT ( 'NONE',  ( -56.88925295215435085, 118.2576901802692646, 47.62393161023230448 ) ) ;
#17412 = CYLINDRICAL_SURFACE ( 'NONE', #2670, 2.000000000000000000 ) ;
#17413 = AXIS2_PLACEMENT_3D ( 'NONE', #18393, #2662, #21804 ) ;
#17414 = CIRCLE ( 'NONE', #14100, 2.000000000000004885 ) ;
#17415 = DIRECTION ( 'NONE',  ( -7.125109674403850657E-05, 0.9999848031710253382, -0.005512562950847868688 ) ) ;
#17416 = DIRECTION ( 'NONE',  ( -0.01292394549866739996, -0.005513023399721131770, -0.9999012842304692006 ) ) ;
#17417 = VERTEX_POINT ( 'NONE', #12090 ) ;
#17418 = CARTESIAN_POINT ( 'NONE',  ( 13.28235005706528682, 159.1720975239875884, 299.5163413053770682 ) ) ;
#17419 = FACE_OUTER_BOUND ( 'NONE', #295, .T. ) ;
#17420 = FACE_OUTER_BOUND ( 'NONE', #12154, .T. ) ;
#17421 = MANIFOLD_SOLID_BREP ( 'Stock-MAS-425-1', #1947 ) ;
#17422 = FACE_OUTER_BOUND ( 'NONE', #6811, .T. ) ;
#17423 = EDGE_CURVE ( 'NONE', #5517, #1302, #4536, .T. ) ;
#17424 = ORIENTED_EDGE ( 'NONE', *, *, #14574, .T. ) ;
#17425 = VECTOR ( 'NONE', #18587, 1000.000000000000114 ) ;
#17426 = CARTESIAN_POINT ( 'NONE',  ( -38.16002667504573509, 95.06337575508095483, 84.40961337517086349 ) ) ;
#17427 = PLANE ( 'NONE',  #8457 ) ;
#17428 = ORIENTED_EDGE ( 'NONE', *, *, #20194, .T. ) ;
#17429 = CARTESIAN_POINT ( 'NONE',  ( -4.162724741132324269, 189.6234579029260487, 275.5491270811696154 ) ) ;
#17430 = ORIENTED_EDGE ( 'NONE', *, *, #5007, .T. ) ;
#17431 = AXIS2_PLACEMENT_3D ( 'NONE', #4634, #9598, #22080 ) ;
#17432 = EDGE_CURVE ( 'NONE', #7572, #9599, #11364, .T. ) ;
#17433 = CARTESIAN_POINT ( 'NONE',  ( -68.43148148480358373, 69.99999999999998579, -86.12277481476654373 ) ) ;
#17434 = VECTOR ( 'NONE', #12343, 999.9999999999998863 ) ;
#17435 = DIRECTION ( 'NONE',  ( 0.9909299940865190504, -0.1338359446631162408, -0.01207007604876292155 ) ) ;
#17436 = SURFACE_STYLE_USAGE ( .BOTH. , #10188 ) ;
#17437 = CARTESIAN_POINT ( 'NONE',  ( 16.93665130137262764, 145.3617413512261010, 276.0582899410866276 ) ) ;
#17438 = EDGE_LOOP ( 'NONE', ( #5227, #7874, #16805, #19408 ) ) ;
#17439 = CARTESIAN_POINT ( 'NONE',  ( 16.39634482804417104, 187.9401017119211019, 319.7988598509799090 ) ) ;
#17440 = ORIENTED_EDGE ( 'NONE', *, *, #22167, .F. ) ;
#17441 = ORIENTED_EDGE ( 'NONE', *, *, #6410, .F. ) ;
#17442 = PLANE ( 'NONE',  #7496 ) ;
#17443 = CARTESIAN_POINT ( 'NONE',  ( 106.5651016638878446, 78.59671595044419234, -27.29699872068776401 ) ) ;
#17444 = ADVANCED_FACE ( 'NONE', ( #18995 ), #6231, .T. ) ;
#17445 = ORIENTED_EDGE ( 'NONE', *, *, #5465, .F. ) ;
#17446 = LINE ( 'NONE', #10428, #20976 ) ;
#17447 = ADVANCED_FACE ( 'NONE', ( #15361 ), #1557, .F. ) ;
#17448 = FACE_BOUND ( 'NONE', #22213, .T. ) ;
#17449 = VERTEX_POINT ( 'NONE', #15585 ) ;
#17450 = DIRECTION ( 'NONE',  ( 0.009985269297354652795, 0.6348858185549770550, 0.7725414498878595548 ) ) ;
#17451 = VERTEX_POINT ( 'NONE', #1449 ) ;
#17452 = CARTESIAN_POINT ( 'NONE',  ( 146.5000000000000000, 18.00000000000000355, -2.025191382850354537E-12 ) ) ;
#17453 = DIRECTION ( 'NONE',  ( -0.01292414190464174703, 0.000000000000000000, -0.9999164797902015955 ) ) ;
#17454 = CARTESIAN_POINT ( 'NONE',  ( 59.68375553853174154, 126.9329139721035489, 168.5814621058240732 ) ) ;
#17455 = COLOUR_RGB ( '', 0.40784314, 0.44705882, 0.49803922) ;
#17456 = ORIENTED_EDGE ( 'NONE', *, *, #18206, .F. ) ;
#17457 = CARTESIAN_POINT ( 'NONE',  ( 20.32642875375586655, 182.3364184945779698, 317.0345009060944221 ) ) ;
#17458 = CARTESIAN_POINT ( 'NONE',  ( 54.52327687265658085, 2.000000000000000000, -111.3697098814019171 ) ) ;
#17459 = EDGE_LOOP ( 'NONE', ( #19882, #22247, #5193, #1392 ) ) ;
#17460 = LINE ( 'NONE', #12168, #8026 ) ;
#17461 = CARTESIAN_POINT ( 'NONE',  ( 48.31072223536619958, 166.8507685304810764, 256.0170097695137201 ) ) ;
#17462 = CARTESIAN_POINT ( 'NONE',  ( 39.99341017485146921, 93.41702043937449673, 83.07303732978165556 ) ) ;
#17463 = DIRECTION ( 'NONE',  ( 0.000000000000000000, -1.000000000000000000, 0.000000000000000000 ) ) ;
#17464 = DIRECTION ( 'NONE',  ( -0.01292394549866632963, -0.005513023399716958026, -0.9999012842304692006 ) ) ;
#17465 = CARTESIAN_POINT ( 'NONE',  ( -146.5000000000000000, 1.999999999999998224, 2.081668171172168513E-14 ) ) ;
#17466 = CARTESIAN_POINT ( 'NONE',  ( -47.94869851243297632, 168.6907664596094776, 35.22912207911639371 ) ) ;
#17467 = AXIS2_PLACEMENT_3D ( 'NONE', #4586, #11614, #18604 ) ;
#17468 = ORIENTED_EDGE ( 'NONE', *, *, #3304, .F. ) ;
#17469 = CARTESIAN_POINT ( 'NONE',  ( -41.83656076456451700, 165.9107905944781862, 244.8766507330992681 ) ) ;
#17470 = PRODUCT_DEFINITION_SHAPE ( 'NONE', 'NONE',  #22667 ) ;
#17471 = CARTESIAN_POINT ( 'NONE',  ( -49.41143953161469682, 111.5125656627889015, -43.54326506131044994 ) ) ;
#17472 = ADVANCED_FACE ( 'NONE', ( #16849 ), #22309, .T. ) ;
#17473 = ORIENTED_EDGE ( 'NONE', *, *, #2125, .F. ) ;
#17474 = CARTESIAN_POINT ( 'NONE',  ( -89.91407985229524513, 87.87209748402599985, 50.86527297701809402 ) ) ;
#17475 = EDGE_LOOP ( 'NONE', ( #7323, #3056, #1517, #428, #8053, #6071 ) ) ;
#17476 = LINE ( 'NONE', #12310, #11423 ) ;
#17477 = CARTESIAN_POINT ( 'NONE',  ( -3.468421381707180728, 158.8820161015420354, 323.7368175311311802 ) ) ;
#17478 = CARTESIAN_POINT ( 'NONE',  ( 51.38234815825343560, 111.9218655255082382, -48.12259961501337102 ) ) ;
#17479 = CARTESIAN_POINT ( 'NONE',  ( -13.92525281995234820, 325.7770340667113942, 328.4523304068723064 ) ) ;
#17480 = FACE_OUTER_BOUND ( 'NONE', #11070, .T. ) ;
#17481 = DIRECTION ( 'NONE',  ( 0.9999164797902015955, 0.000000000000000000, -0.01292414190463697134 ) ) ;
#17482 = EDGE_LOOP ( 'NONE', ( #12326, #15703, #9358, #22597 ) ) ;
#17483 = CARTESIAN_POINT ( 'NONE',  ( -0.5919341415252730165, 327.2293163420105770, 310.4847058774875563 ) ) ;
#17484 = ORIENTED_EDGE ( 'NONE', *, *, #2623, .F. ) ;
#17485 = CARTESIAN_POINT ( 'NONE',  ( 28.96536656690224021, 99.74539563421257071, 74.50764472524521409 ) ) ;
#17486 = ADVANCED_FACE ( 'NONE', ( #4643 ), #11562, .F. ) ;
#17487 = CARTESIAN_POINT ( 'NONE',  ( -89.55253866421617204, 89.09534416471163354, 51.72748700526515364 ) ) ;
#17489 = ORIENTED_EDGE ( 'NONE', *, *, #3252, .T. ) ;
#17488 = ORIENTED_EDGE ( 'NONE', *, *, #3273, .F. ) ;
#17490 = ORIENTED_EDGE ( 'NONE', *, *, #9376, .T. ) ;
#17491 = DIRECTION ( 'NONE',  ( 0.8981428216242088869, -0.000000000000000000, -0.4397038457472309814 ) ) ;
#17492 = DIRECTION ( 'NONE',  ( 0.01292394549866737220, 0.005513023399721000799, 0.9999012842304692006 ) ) ;
#17493 = ORIENTED_EDGE ( 'NONE', *, *, #22453, .F. ) ;
#17494 = DIRECTION ( 'NONE',  ( 0.3101392564284310982, 0.9506461370142479383, -0.009250070373107712254 ) ) ;
#17495 = CYLINDRICAL_SURFACE ( 'NONE', #13143, 3.399999999999986144 ) ;
#17496 = CARTESIAN_POINT ( 'NONE',  ( 52.66525871368118317, 166.9576235287527481, 267.9613219752613418 ) ) ;
#17497 = CYLINDRICAL_SURFACE ( 'NONE', #6001, 102.6746853779045381 ) ;
#17498 = EDGE_LOOP ( 'NONE', ( #3157, #200, #7088, #12388 ) ) ;
#17499 = ORIENTED_EDGE ( 'NONE', *, *, #17786, .T. ) ;
#17500 = DIRECTION ( 'NONE',  ( -2.025474946048326158E-22, 1.000000000000000000, -1.876735158486679638E-22 ) ) ;
#17501 = CARTESIAN_POINT ( 'NONE',  ( -75.17629230947522956, 75.01375443481772720, -0.6738748282868175510 ) ) ;
#17502 = CARTESIAN_POINT ( 'NONE',  ( -7.771066633828587200, 165.4076424879065996, 321.2562038772189226 ) ) ;
#17503 = ADVANCED_FACE ( 'NONE', ( #8107 ), #20489, .F. ) ;
#17504 = EDGE_CURVE ( 'NONE', #2673, #14965, #14322, .T. ) ;
#17505 = DIRECTION ( 'NONE',  ( 7.125109674364536131E-05, -0.9999848031710253382, 0.005512562950849705760 ) ) ;
#17506 = ORIENTED_EDGE ( 'NONE', *, *, #14081, .T. ) ;
#17507 = CARTESIAN_POINT ( 'NONE',  ( -38.21725235583850377, 94.02752048664900997, -82.48544352224706699 ) ) ;
#17508 = DIRECTION ( 'NONE',  ( -0.9999164797902015955, -2.044556590511377167E-15, 0.01292414190464178346 ) ) ;
#17509 = EDGE_LOOP ( 'NONE', ( #17046, #19975, #12633, #807 ) ) ;
#17510 = ORIENTED_EDGE ( 'NONE', *, *, #4314, .T. ) ;
#17511 =( BOUNDED_SURFACE ( )  B_SPLINE_SURFACE ( 3, 2, ( 
 ( #7737, #19774, #393 ),
 ( #4273, #862, #740 ),
 ( #21831, #11075, #14774 ),
 ( #11297, #624, #9577 ) ),
 .UNSPECIFIED., .F., .F., .T. ) 
 B_SPLINE_SURFACE_WITH_KNOTS ( ( 4, 4 ),
 ( 3, 3 ),
 ( 0.4226013619543069755, 0.4841788640348455575 ),
 ( 0.000000000000000000, 1.000000000000000000 ),
 .UNSPECIFIED. ) 
 GEOMETRIC_REPRESENTATION_ITEM ( )  RATIONAL_B_SPLINE_SURFACE ( (
 ( 1.000000000000000000, 0.9068900557993654354, 1.000000000000000000),
 ( 1.000000000000000000, 0.9052491015987682577, 1.000000000000000000),
 ( 1.000000000000000000, 0.9034913259101550187, 1.000000000000000000),
 ( 1.000000000000000000, 0.9016180287879269617, 1.000000000000000000) ) ) 
 REPRESENTATION_ITEM ( '' )  SURFACE ( )  );
#17512 = DIRECTION ( 'NONE',  ( -0.9999164797902015955, -6.938893903907235477E-15, 0.01292414190464525985 ) ) ;
#17513 = EDGE_LOOP ( 'NONE', ( #4521, #5176, #18811, #8796 ) ) ;
#17514 = ORIENTED_EDGE ( 'NONE', *, *, #2926, .T. ) ;
#17515 = VERTEX_POINT ( 'NONE', #17296 ) ;
#17516 = ADVANCED_FACE ( 'NONE', ( #2928 ), #22090, .T. ) ;
#17517 = CARTESIAN_POINT ( 'NONE',  ( 17.86990006708586165, 186.2024540464122708, 309.9547898294551942 ) ) ;
#17518 = VERTEX_POINT ( 'NONE', #13628 ) ;
#17519 = AXIS2_PLACEMENT_3D ( 'NONE', #18037, #9286, #21552 ) ;
#17520 = EDGE_CURVE ( 'NONE', #3243, #9760, #19060, .T. ) ;
#17521 = FACE_OUTER_BOUND ( 'NONE', #22497, .T. ) ;
#17522 = CARTESIAN_POINT ( 'NONE',  ( -90.92043330041786930, 70.33842041176643534, 61.91522761515599882 ) ) ;
#17523 = DIRECTION ( 'NONE',  ( -0.9999164797902017066, -2.001050586450178931E-22, 0.01292414190464131508 ) ) ;
#17524 = CARTESIAN_POINT ( 'NONE',  ( -40.94568735521033886, 95.78253051705814869, 82.61534438928066493 ) ) ;
#17525 = DIRECTION ( 'NONE',  ( -0.01292414190464137060, 0.000000000000000000, -0.9999164797902015955 ) ) ;
#17526 = CARTESIAN_POINT ( 'NONE',  ( 85.57356156445646889, 75.03970044275367002, -3.878440373465425139 ) ) ;
#17527 = CARTESIAN_POINT ( 'NONE',  ( 13.57515324494882769, 187.0243046317364701, 305.1469784402785308 ) ) ;
#17528 = CARTESIAN_POINT ( 'NONE',  ( 91.24493283426487267, 78.25381457448439448, 30.56897831620030459 ) ) ;
#17529 = MANIFOLD_SOLID_BREP ( 'Stock-MAS-425-1', #6212 ) ;
#17530 = EDGE_CURVE ( 'NONE', #7441, #2301, #6249, .T. ) ;
#17531 = CARTESIAN_POINT ( 'NONE',  ( 89.24601225622841127, 80.14389198580501272, 29.68648583522423934 ) ) ;
#17532 = EDGE_LOOP ( 'NONE', ( #14401, #3973, #21795, #10841 ) ) ;
#17533 = EDGE_CURVE ( 'NONE', #5229, #4135, #17782, .T. ) ;
#17534 = CONICAL_SURFACE ( 'NONE', #3186, 3.399999999999986144, 1.029744258676653201 ) ;
#17535 = CARTESIAN_POINT ( 'NONE',  ( -10.85595612533484911, 109.6999345499266525, 127.2773526115149281 ) ) ;
#17536 = CARTESIAN_POINT ( 'NONE',  ( 10.89474438599883221, 174.2127514147958891, 324.4667421121108646 ) ) ;
#17537 = VERTEX_POINT ( 'NONE', #21283 ) ;
#17538 = CARTESIAN_POINT ( 'NONE',  ( -91.85896106039054132, 79.10764833873336954, -26.44817522613631411 ) ) ;
#17539 = ORIENTED_EDGE ( 'NONE', *, *, #14726, .T. ) ;
#17540 = EDGE_LOOP ( 'NONE', ( #11582, #20983, #9596, #18937, #6405, #21873, #2978, #2890, #7066, #6229 ) ) ;
#17541 = CARTESIAN_POINT ( 'NONE',  ( -68.70320840996376432, 69.99999999999998579, -85.90686588605387897 ) ) ;
#17542 = ADVANCED_FACE ( 'NONE', ( #8999 ), #13235, .F. ) ;
#17543 = PRODUCT_DEFINITION_CONTEXT ( 'detailed design', #13667, 'design' ) ;
#17544 = DIRECTION ( 'NONE',  ( 0.000000000000000000, 0.000000000000000000, -1.000000000000000000 ) ) ;
#17546 = FACE_OUTER_BOUND ( 'NONE', #9331, .T. ) ;
#17545 = AXIS2_PLACEMENT_3D ( 'NONE', #20096, #4361, #7490 ) ;
#17547 = DIRECTION ( 'NONE',  ( 7.125109674364536131E-05, -0.9999848031710253382, 0.005512562950849705760 ) ) ;
#17548 = FACE_OUTER_BOUND ( 'NONE', #6554, .T. ) ;
#17549 = ORIENTED_EDGE ( 'NONE', *, *, #17947, .T. ) ;
#17550 = DIRECTION ( 'NONE',  ( -5.440186201345739411E-18, -1.000000000000000000, -1.334940939666364181E-17 ) ) ;
#17551 = ORIENTED_EDGE ( 'NONE', *, *, #7404, .T. ) ;
#17552 = ORIENTED_EDGE ( 'NONE', *, *, #7956, .F. ) ;
#17553 = DIRECTION ( 'NONE',  ( -0.9999164797902015955, -6.965998958219364448E-18, 0.01292414190464157182 ) ) ;
#17554 = ADVANCED_FACE ( 'NONE', ( #22634 ), #19965, .F. ) ;
#17555 = CARTESIAN_POINT ( 'NONE',  ( 50.89493962932122173, 107.8908830597778064, 68.91667391595403558 ) ) ;
#17556 = DIRECTION ( 'NONE',  ( -0.01292394549866745720, -0.005513023399720816918, -0.9999012842304692006 ) ) ;
#17557 = CARTESIAN_POINT ( 'NONE',  ( 146.5000000000000000, 1.999999999999998224, -2.025191382850354537E-12 ) ) ;
#17558 = ORIENTED_EDGE ( 'NONE', *, *, #475, .T. ) ;
#17559 = CONICAL_SURFACE ( 'NONE', #9843, 5.700000000000003730, 0.7853981633974482790 ) ;
#17560 = FACE_OUTER_BOUND ( 'NONE', #21069, .T. ) ;
#17561 = CARTESIAN_POINT ( 'NONE',  ( -90.46801631146684031, 78.10499069285114615, 32.69910015975905537 ) ) ;
#17562 = CARTESIAN_POINT ( 'NONE',  ( -5.817627660042380633, 326.6189945014031082, 307.3338991736922594 ) ) ;
#17563 = CARTESIAN_POINT ( 'NONE',  ( -15.23311339992631197, 178.2575602159987227, 317.4829393096611625 ) ) ;
#17564 = MANIFOLD_SOLID_BREP ( 'Stock-MAS-425-1', #347 ) ;
#17565 = VECTOR ( 'NONE', #12484, 999.9999999999998863 ) ;
#17566 = CARTESIAN_POINT ( 'NONE',  ( 13.80207227627342803, 186.9166813556422255, 305.2099784584296458 ) ) ;
#17567 = DIRECTION ( 'NONE',  ( 7.125109674403277385E-05, -0.9999848031710253382, 0.005512562950848281552 ) ) ;
#17568 = ORIENTED_EDGE ( 'NONE', *, *, #19955, .F. ) ;
#17569 = CARTESIAN_POINT ( 'NONE',  ( -1.163172771417702700, 81.99999999999998579, -89.99248318111824574 ) ) ;
#17570 = EDGE_CURVE ( 'NONE', #822, #7475, #8432, .T. ) ;
#17571 = CONTEXT_DEPENDENT_SHAPE_REPRESENTATION ( #17811, #4962 ) ;
#17572 = EDGE_CURVE ( 'NONE', #10802, #13612, #5664, .T. ) ;
#17573 = CARTESIAN_POINT ( 'NONE',  ( 59.65023440614042727, 143.9188730675116688, 165.9879953250834603 ) ) ;
#17574 = AXIS2_PLACEMENT_3D ( 'NONE', #14888, #21830, #15102 ) ;
#17575 = ORIENTED_EDGE ( 'NONE', *, *, #20428, .F. ) ;
#17576 = CARTESIAN_POINT ( 'NONE',  ( -50.73053929929668726, 108.7816493830516151, -43.51115831301089543 ) ) ;
#17577 = DIRECTION ( 'NONE',  ( -0.9934404589540162256, -0.1135548637187057258, 0.01346653032743021748 ) ) ;
#17578 = DIRECTION ( 'NONE',  ( -0.01292394549866743465, -0.005513023399721021615, -0.9999012842304692006 ) ) ;
#17579 = PRESENTATION_LAYER_ASSIGNMENT (  '', '', ( #9496 ) ) ;
#17580 = DIRECTION ( 'NONE',  ( 0.01035335185279151644, 0.005513005182360133580, 0.9999312050732649393 ) ) ;
#17581 = ORIENTED_EDGE ( 'NONE', *, *, #21490, .T. ) ;
#17582 = FACE_OUTER_BOUND ( 'NONE', #10701, .T. ) ;
#17583 = DIRECTION ( 'NONE',  ( -0.01292394549866632963, -0.005513023399716958026, -0.9999012842304692006 ) ) ;
#17584 = ORIENTED_EDGE ( 'NONE', *, *, #20019, .T. ) ;
#17585 = CARTESIAN_POINT ( 'NONE',  ( -89.40156491642460423, 88.37278921414913668, 50.55266491976622945 ) ) ;
#17586 = VERTEX_POINT ( 'NONE', #3938 ) ;
#17587 = CARTESIAN_POINT ( 'NONE',  ( 106.3651776870870691, 78.54983655346507021, 28.04389441634570446 ) ) ;
#17588 = CARTESIAN_POINT ( 'NONE',  ( -90.17351897532782345, 87.00751446224754204, 51.38173066951565460 ) ) ;
#17589 = DIRECTION ( 'NONE',  ( 0.01292394549866738782, 0.005513023399720700692, 0.9999012842304693116 ) ) ;
#17590 = VERTEX_POINT ( 'NONE', #6126 ) ;
#17591 = LINE ( 'NONE', #3331, #2701 ) ;
#17592 = CARTESIAN_POINT ( 'NONE',  ( -1.163172771417702478, 87.00000000000001421, -89.99248318111824574 ) ) ;
#17593 = VECTOR ( 'NONE', #2007, 1000.000000000000114 ) ;
#17594 = CARTESIAN_POINT ( 'NONE',  ( 17.20172502694573780, 168.2615119090760345, 320.7598891025185708 ) ) ;
#17595 = DIRECTION ( 'NONE',  ( -0.01292394549866731843, -0.005513023399720594006, -0.9999012842304693116 ) ) ;
#17596 = CIRCLE ( 'NONE', #19407, 6.500000000000000000 ) ;
#17597 = EDGE_LOOP ( 'NONE', ( #11355, #14849, #17752, #755 ) ) ;
#17598 = CARTESIAN_POINT ( 'NONE',  ( -65.67129704762463405, 144.7109461922390778, -51.51693412452669918 ) ) ;
#17599 = EDGE_CURVE ( 'NONE', #4965, #2088, #18429, .T. ) ;
#17600 = CARTESIAN_POINT ( 'NONE',  ( -89.87306261084498260, 88.90191489356698185, 52.23091996317439367 ) ) ;
#17601 = ORIENTED_EDGE ( 'NONE', *, *, #514, .F. ) ;
#17602 = ORIENTED_EDGE ( 'NONE', *, *, #4275, .F. ) ;
#17603 = CARTESIAN_POINT ( 'NONE',  ( -92.46788464407291031, 79.04398536104955042, 28.62013883513304080 ) ) ;
#17604 = CARTESIAN_POINT ( 'NONE',  ( -34.68008326079426951, 93.81386119346835528, 83.23154952960750563 ) ) ;
#17605 = ORIENTED_EDGE ( 'NONE', *, *, #4609, .F. ) ;
#17606 = CONICAL_SURFACE ( 'NONE', #7684, 2.499999999999988010, 1.029744258676651425 ) ;
#17607 = CARTESIAN_POINT ( 'NONE',  ( -91.21019055468684655, 77.12912189496638860, -28.82359390673209631 ) ) ;
#17608 = VECTOR ( 'NONE', #1342, 999.9999999999998863 ) ;
#17609 = CARTESIAN_POINT ( 'NONE',  ( 1.080781817686064405, 165.4609577950973573, 83.61805050855254251 ) ) ;
#17610 = ORIENTED_EDGE ( 'NONE', *, *, #16872, .F. ) ;
#17611 = CARTESIAN_POINT ( 'NONE',  ( -1.247179693797872524, 69.99999999999998579, -96.49194029975447506 ) ) ;
#17612 = EDGE_LOOP ( 'NONE', ( #6815, #1102, #19950, #2544, #20821, #13619, #19102, #7688, #19377, #16364, #18279, #21923, #13866, #10683, #14734, #4578, #982, #11060, #10129, #21566, #11491 ) ) ;
#17613 = CARTESIAN_POINT ( 'NONE',  ( 1.717753310876221295, 45.00000000000000000, 109.6869605904137330 ) ) ;
#17614 = CARTESIAN_POINT ( 'NONE',  ( -77.24079330402096843, 75.09876982897525011, 5.330581268580301568 ) ) ;
#17615 = CARTESIAN_POINT ( 'NONE',  ( -11.16028402830248289, 165.0151156927683473, 320.0325255541022784 ) ) ;
#17616 = CARTESIAN_POINT ( 'NONE',  ( -105.4334892372614121, 77.12912189496637438, 31.36525700924958926 ) ) ;
#17617 = DIRECTION ( 'NONE',  ( -0.7069973413461592138, -0.7070960354057278519, 0.01303671902605246964 ) ) ;
#17618 = DIRECTION ( 'NONE',  ( -0.01292394549866632963, -0.005513023399716958026, -0.9999012842304692006 ) ) ;
#17619 = CARTESIAN_POINT ( 'NONE',  ( -49.61330349940486428, 114.6621811589122757, 166.8870046147178812 ) ) ;
#17620 = ORIENTED_EDGE ( 'NONE', *, *, #20725, .F. ) ;
#17621 = CARTESIAN_POINT ( 'NONE',  ( -49.64892827247505380, 126.1473081376431367, 27.48487435773119714 ) ) ;
#17622 = ORIENTED_EDGE ( 'NONE', *, *, #13196, .T. ) ;
#17623 = AXIS2_PLACEMENT_3D ( 'NONE', #17104, #20749, #1366 ) ;
#17624 = VERTEX_POINT ( 'NONE', #18103 ) ;
#17625 = EDGE_CURVE ( 'NONE', #3455, #17005, #11197, .T. ) ;
#17626 = AXIS2_PLACEMENT_3D ( 'NONE', #5553, #7392, #2223 ) ;
#17627 = APPLICATION_CONTEXT ( 'automotive_design' ) ;
#17628 = CARTESIAN_POINT ( 'NONE',  ( 19.80886166575337981, 183.6751623284734194, 313.1938135270697785 ) ) ;
#17629 = EDGE_CURVE ( 'NONE', #9497, #3176, #20463, .T. ) ;
#17630 = VERTEX_POINT ( 'NONE', #4387 ) ;
#17631 = CONICAL_SURFACE ( 'NONE', #4030, 15.00000000000000533, 0.03490658503988662564 ) ;
#17632 = CYLINDRICAL_SURFACE ( 'NONE', #19737, 2.000000000000001332 ) ;
#17633 = DIRECTION ( 'NONE',  ( 0.9999164797902017066, 6.965998958219365988E-18, -0.01292414190464157356 ) ) ;
#17634 = ADVANCED_FACE ( 'NONE', ( #2573, #5895 ), #21503, .T. ) ;
#17635 = DIRECTION ( 'NONE',  ( 0.5089394657577702707, 0.004781488884709769391, 0.8607890319690654213 ) ) ;
#17636 = DIRECTION ( 'NONE',  ( 0.01292394549866734098, 0.005513023399720419666, 0.9999012842304692006 ) ) ;
#17637 = CARTESIAN_POINT ( 'NONE',  ( -38.94547111459952760, 95.87640844880095869, 82.49456443487720492 ) ) ;
#17638 = ORIENTED_EDGE ( 'NONE', *, *, #20789, .T. ) ;
#17639 = CARTESIAN_POINT ( 'NONE',  ( 80.72863657406642801, 75.20316443938568796, -7.254142036499096946 ) ) ;
#17640 = CARTESIAN_POINT ( 'NONE',  ( 13.39998349785021681, 190.1428121419461093, 307.9026663383229447 ) ) ;
#17641 = DIRECTION ( 'NONE',  ( 0.9999164797902015955, 6.965998958219364448E-18, -0.01292414190464157182 ) ) ;
#17642 = CIRCLE ( 'NONE', #5878, 8.000000000000000000 ) ;
#17643 = CIRCLE ( 'NONE', #12506, 7.500000000000002665 ) ;
#17644 = EDGE_CURVE ( 'NONE', #20719, #19509, #16887, .T. ) ;
#17645 = CARTESIAN_POINT ( 'NONE',  ( 4.182528737366220106, 166.7840834110302808, 323.5943587238651276 ) ) ;
#17646 = ORIENTED_EDGE ( 'NONE', *, *, #7815, .T. ) ;
#17647 =( LENGTH_UNIT ( ) NAMED_UNIT ( * ) SI_UNIT ( .MILLI., .METRE. ) );
#17648 = EDGE_CURVE ( 'NONE', #6364, #3254, #10287, .T. ) ;
#17649 = CIRCLE ( 'NONE', #15830, 3.047499999999998987 ) ;
#17650 =( BOUNDED_CURVE ( )  B_SPLINE_CURVE ( 3, ( #2278, #21653, #9277, #12634 ),
 .UNSPECIFIED., .F., .T. ) 
 B_SPLINE_CURVE_WITH_KNOTS ( ( 4, 4 ),
 ( 5.433035758877963417, 5.587168164874065646 ),
 .UNSPECIFIED. ) 
 CURVE ( )  GEOMETRIC_REPRESENTATION_ITEM ( )  RATIONAL_B_SPLINE_CURVE ( ( 1.000000000000000000, 0.9980212464270939998, 0.9980212464270939998, 1.000000000000000000 ) ) 
 REPRESENTATION_ITEM ( '' )  );
#17651 = AXIS2_PLACEMENT_3D ( 'NONE', #544, #13078, #18456 ) ;
#17652 = EDGE_CURVE ( 'NONE', #15977, #558, #17985, .T. ) ;
#17653 = CARTESIAN_POINT ( 'NONE',  ( -9.157834647979710141, 186.7064098873641456, 321.4482401296887701 ) ) ;
#17654 = AXIS2_PLACEMENT_3D ( 'NONE', #1351, #22320, #3264 ) ;
#17655 = PLANE ( 'NONE',  #7745 ) ;
#17656 = ORIENTED_EDGE ( 'NONE', *, *, #22228, .F. ) ;
#17657 = CARTESIAN_POINT ( 'NONE',  ( -91.52774025374972666, 80.10656073859030357, -29.55378794065120474 ) ) ;
#17658 = VERTEX_POINT ( 'NONE', #21398 ) ;
#17659 = EDGE_CURVE ( 'NONE', #18018, #2060, #9228, .T. ) ;
#17660 = PRODUCT_DEFINITION_SHAPE ( 'NONE', 'NONE',  #22691 ) ;
#17661 = AXIS2_PLACEMENT_3D ( 'NONE', #19119, #14325, #19352 ) ;
#17662 = CARTESIAN_POINT ( 'NONE',  ( -6.632709584382732615, 70.55846734465490044, -81.62749566292762893 ) ) ;
#17663 = EDGE_CURVE ( 'NONE', #14769, #12640, #13053, .T. ) ;
#17664 = CIRCLE ( 'NONE', #18388, 8.000000000000014211 ) ;
#17665 = DIRECTION ( 'NONE',  ( 5.440186201345738641E-18, 1.000000000000000000, 1.334940939666364181E-17 ) ) ;
#17666 = ORIENTED_EDGE ( 'NONE', *, *, #11361, .F. ) ;
#17667 = EDGE_CURVE ( 'NONE', #18283, #126, #19783, .T. ) ;
#17668 = CARTESIAN_POINT ( 'NONE',  ( -44.54898248114584192, 168.6907664596095913, 35.18517999664060625 ) ) ;
#17669 = CYLINDRICAL_SURFACE ( 'NONE', #4131, 4.200000000000005507 ) ;
#17670 = COLOUR_RGB ( '', 0.09019608, 0.27058824, 0.51372549) ;
#17671 = VERTEX_POINT ( 'NONE', #626 ) ;
#17672 = CARTESIAN_POINT ( 'NONE',  ( 12.31279916714637146, 188.3155709156417856, 320.9502181276351962 ) ) ;
#17673 = ORIENTED_EDGE ( 'NONE', *, *, #13060, .F. ) ;
#17674 = DIRECTION ( 'NONE',  ( 0.9999164797902017066, 2.001050586450178931E-22, -0.01292414190464131508 ) ) ;
#17675 = CARTESIAN_POINT ( 'NONE',  ( -39.42082737383935154, 72.00000000000000000, 83.51645567887779009 ) ) ;
#17676 = EDGE_CURVE ( 'NONE', #7464, #11795, #516, .T. ) ;
#17677 = CARTESIAN_POINT ( 'NONE',  ( 2.067862704742617463, 72.00000000000000000, 159.9866367664322979 ) ) ;
#17678 = ORIENTED_EDGE ( 'NONE', *, *, #451, .T. ) ;
#17679 = CARTESIAN_POINT ( 'NONE',  ( -8.521464884669340378, 185.2469399555467646, 323.2491637953797863 ) ) ;
#17680 = DIRECTION ( 'NONE',  ( -0.01292414190464137060, 8.764918615461757854E-16, -0.9999164797902015955 ) ) ;
#17681 = CARTESIAN_POINT ( 'NONE',  ( 44.03052579490771024, 164.6879759653328961, -75.29719582347730977 ) ) ;
#17682 = VERTEX_POINT ( 'NONE', #7516 ) ;
#17683 = CARTESIAN_POINT ( 'NONE',  ( -10.63979810906646328, 187.2538219846114487, 308.2525677622306830 ) ) ;
#17684 = VECTOR ( 'NONE', #16259, 999.9999999999998863 ) ;
#17685 = EDGE_CURVE ( 'NONE', #3794, #6936, #20116, .T. ) ;
#17686 = PRODUCT_DEFINITION_SHAPE ( 'NONE', 'NONE',  #20803 ) ;
#17687 = CARTESIAN_POINT ( 'NONE',  ( -44.75629999235007972, 176.1024441089967638, 19.14541522682172925 ) ) ;
#17688 = DIRECTION ( 'NONE',  ( 7.125109674160258889E-05, -0.9999848031710252272, 0.005512562950849897447 ) ) ;
#17689 = CARTESIAN_POINT ( 'NONE',  ( -15.31456691273178450, 178.2055753609038220, 312.1839202388429726 ) ) ;
#17690 = AXIS2_PLACEMENT_3D ( 'NONE', #20799, #22278, #8508 ) ;
#17691 = CARTESIAN_POINT ( 'NONE',  ( 17.16753617371702134, 177.4987173824078468, 90.22667393302013750 ) ) ;
#17692 = CIRCLE ( 'NONE', #809, 22.49999999999999645 ) ;
#17693 = CARTESIAN_POINT ( 'NONE',  ( 49.42384346307601106, 125.7553391191873544, -44.89926147365057574 ) ) ;
#17694 = EDGE_CURVE ( 'NONE', #2170, #6548, #18698, .T. ) ;
#17695 = ITEM_DEFINED_TRANSFORMATION ( 'NONE', 'NONE', #21995,  #6292 ) ;
#17696 = VECTOR ( 'NONE', #22123, 1000.000000000000114 ) ;
#17697 = VECTOR ( 'NONE', #20924, 1000.000000000000114 ) ;
#17698 = LINE ( 'NONE', #10792, #12230 ) ;
#17699 = CYLINDRICAL_SURFACE ( 'NONE', #2966, 3.399999999999992806 ) ;
#17700 = LINE ( 'NONE', #9160, #12971 ) ;
#17701 = VECTOR ( 'NONE', #6653, 1000.000000000000000 ) ;
#17702 = ORIENTED_EDGE ( 'NONE', *, *, #20307, .F. ) ;
#17703 = CARTESIAN_POINT ( 'NONE',  ( 1.236893267138826732E-14, 37.00000000000000711, 101.0000000000000000 ) ) ;
#17704 = CARTESIAN_POINT ( 'NONE',  ( -51.12457683484994675, 113.1366485501290953, -43.53007687325056452 ) ) ;
#17705 = VERTEX_POINT ( 'NONE', #21610 ) ;
#17706 = DIRECTION ( 'NONE',  ( 0.01292414190464177652, 1.902755938799532355E-22, 0.9999164797902015955 ) ) ;
#17707 = AXIS2_PLACEMENT_3D ( 'NONE', #18066, #250, #12429 ) ;
#17708 = ORIENTED_EDGE ( 'NONE', *, *, #11636, .F. ) ;
#17709 = DIRECTION ( 'NONE',  ( 0.8981428216242086648, 1.300010802462040013E-16, -0.4397038457472312589 ) ) ;
#17710 = DIRECTION ( 'NONE',  ( 5.440186201345738641E-18, 1.000000000000000000, 1.334940939666364181E-17 ) ) ;
#17711 = PLANE ( 'NONE',  #5564 ) ;
#17712 = ORIENTED_EDGE ( 'NONE', *, *, #15505, .F. ) ;
#17713 = ADVANCED_FACE ( 'NONE', ( #19900 ), #4170, .F. ) ;
#17714 = DIRECTION ( 'NONE',  ( -0.01292394549866731843, -0.005513023399720594006, -0.9999012842304693116 ) ) ;
#17715 = DIRECTION ( 'NONE',  ( -0.01292394549866740863, -0.005513023399721009472, -0.9999012842304692006 ) ) ;
#17716 = AXIS2_PLACEMENT_3D ( 'NONE', #22469, #22354, #3093 ) ;
#17717 = VECTOR ( 'NONE', #20996, 999.9999999999998863 ) ;
#17718 = AXIS2_PLACEMENT_3D ( 'NONE', #9367, #19801, #16934 ) ;
#17719 = CARTESIAN_POINT ( 'NONE',  ( 20.34336355497194049, 168.6127106875439381, 318.7583842999745229 ) ) ;
#17720 = ORIENTED_EDGE ( 'NONE', *, *, #10468, .F. ) ;
#17721 = CARTESIAN_POINT ( 'NONE',  ( 90.45626474936497630, 70.75678324216411852, -62.59145595768703174 ) ) ;
#17722 = CARTESIAN_POINT ( 'NONE',  ( -89.69275295551862826, 89.03869477057148174, 51.93053011967995758 ) ) ;
#17723 = CIRCLE ( 'NONE', #7797, 25.50000000000000000 ) ;
#17725 = ORIENTED_EDGE ( 'NONE', *, *, #14168, .F. ) ;
#17724 = ORIENTED_EDGE ( 'NONE', *, *, #3050, .F. ) ;
#17726 = ORIENTED_EDGE ( 'NONE', *, *, #6704, .T. ) ;
#17727 = CARTESIAN_POINT ( 'NONE',  ( -36.80549447617401881, 105.5072037373731888, 92.66220808178287882 ) ) ;
#17728 = DIRECTION ( 'NONE',  ( -0.000000000000000000, 1.000000000000000000, -0.000000000000000000 ) ) ;
#17729 = FILL_AREA_STYLE ('',( #9189 ) ) ;
#17730 = CIRCLE ( 'NONE', #2684, 3.309500000000002107 ) ;
#17731 = CARTESIAN_POINT ( 'NONE',  ( 80.72971245143067165, 75.13518351147561702, 4.023615192978592603 ) ) ;
#17732 = AXIS2_PLACEMENT_3D ( 'NONE', #16253, #2674, #2327 ) ;
#17733 = LINE ( 'NONE', #253, #16114 ) ;
#17734 = B_SPLINE_CURVE_WITH_KNOTS ( 'NONE', 3,
 ( #10117, #15525, #22478, #4473, #7222, #22584, #5514, #10801, #17471, #6993, #3318, #3441, #14143, #3657, #17704, #5030, #12064, #13897, #14251, #3779 ),
 .UNSPECIFIED., .F., .F.,
 ( 4, 2, 2, 2, 2, 2, 2, 2, 2, 4 ),
 ( 0.000000000000000000, 0.0008942227389302294686, 0.001788445477860458937, 0.002682668216790688731, 0.003576890955720917874, 0.004471113694651147018, 0.005365336433581377462, 0.005812447803046480975, 0.006259559172511584488, 0.007153781911441802789 ),
 .UNSPECIFIED. ) ;
#17735 = FACE_OUTER_BOUND ( 'NONE', #8530, .T. ) ;
#17736 = ORIENTED_EDGE ( 'NONE', *, *, #8086, .T. ) ;
#17737 = B_SPLINE_CURVE_WITH_KNOTS ( 'NONE', 3,
 ( #20943, #21173, #5204, #12238, #15065, #20200, #6440, #21797, #20424, #4678, #16894, #7925, #18600, #16787, #13114, #22023 ),
 .UNSPECIFIED., .F., .F.,
 ( 4, 2, 2, 2, 2, 2, 2, 4 ),
 ( 0.000000000000000000, 0.0004291333152394394778, 0.0008582666304788767872, 0.001716533260957743600, 0.002145666576197192889, 0.002574799891436641529, 0.003003933206676090602, 0.003433066521915540108 ),
 .UNSPECIFIED. ) ;
#17738 = CARTESIAN_POINT ( 'NONE',  ( 153.9999999999992610, 1.999999999999998224, 53.76161406891468175 ) ) ;
#17739 = ORIENTED_EDGE ( 'NONE', *, *, #2894, .F. ) ;
#17740 = DIRECTION ( 'NONE',  ( 7.125109674403838460E-05, -0.9999848031710254492, 0.005512562950847868688 ) ) ;
#17741 = DIRECTION ( 'NONE',  ( -0.9999164797902015955, -6.965998958219364448E-18, 0.01292414190464157182 ) ) ;
#17742 = LINE ( 'NONE', #1987, #15332 ) ;
#17743 = CARTESIAN_POINT ( 'NONE',  ( -11.79244185255453203, 164.9406916783147494, 319.5044911414121884 ) ) ;
#17744 = EDGE_CURVE ( 'NONE', #7438, #1225, #17154, .T. ) ;
#17745 = VERTEX_POINT ( 'NONE', #15107 ) ;
#17746 = DIRECTION ( 'NONE',  ( -0.9999164797902017066, -2.001050586450178931E-22, 0.01292414190464131508 ) ) ;
#17747 = ADVANCED_FACE ( 'NONE', ( #17057 ), #2211, .T. ) ;
#17748 = CARTESIAN_POINT ( 'NONE',  ( -14.53239793090661180, 175.6255473142593644, 113.6490011371711688 ) ) ;
#17749 =( NAMED_UNIT ( * ) PLANE_ANGLE_UNIT ( ) SI_UNIT ( $, .RADIAN. ) );
#17750 = EDGE_CURVE ( 'NONE', #12076, #21601, #14992, .T. ) ;
#17751 = CARTESIAN_POINT ( 'NONE',  ( -49.89972388002872350, 114.5241193755163209, 166.5137936661477909 ) ) ;
#17752 = ORIENTED_EDGE ( 'NONE', *, *, #11482, .T. ) ;
#17753 = FACE_OUTER_BOUND ( 'NONE', #11920, .T. ) ;
#17754 = ORIENTED_EDGE ( 'NONE', *, *, #19715, .F. ) ;
#17755 = CIRCLE ( 'NONE', #3423, 2.000000000000001332 ) ;
#17756 = ORIENTED_EDGE ( 'NONE', *, *, #1984, .T. ) ;
#17757 = ORIENTED_EDGE ( 'NONE', *, *, #10529, .F. ) ;
#17758 = CIRCLE ( 'NONE', #19907, 3.099999999999998757 ) ;
#17759 = DIRECTION ( 'NONE',  ( -0.01104128644981183967, -0.5197558313507629757, -0.8542435049623791077 ) ) ;
#17760 = ORIENTED_EDGE ( 'NONE', *, *, #10761, .T. ) ;
#17761 = FACE_OUTER_BOUND ( 'NONE', #3590, .T. ) ;
#17762 = CARTESIAN_POINT ( 'NONE',  ( 41.28420658616847305, 94.99786382055521017, -44.62447144312741898 ) ) ;
#17763 = CARTESIAN_POINT ( 'NONE',  ( -88.05170339851980543, 72.97786998644572520, 61.56719313945616534 ) ) ;
#17764 = VECTOR ( 'NONE', #1235, 1000.000000000000227 ) ;
#17765 = CYLINDRICAL_SURFACE ( 'NONE', #4158, 8.000000000000003553 ) ;
#17766 = CARTESIAN_POINT ( 'NONE',  ( 3.603563735215878250, 86.00000000000001421, -86.34855356100663926 ) ) ;
#17767 = CARTESIAN_POINT ( 'NONE',  ( -38.64445966580888836, 96.64268400674895076, 84.48542380140278851 ) ) ;
#17768 = DIRECTION ( 'NONE',  ( 0.000000000000000000, 0.000000000000000000, 1.000000000000000000 ) ) ;
#17769 = CARTESIAN_POINT ( 'NONE',  ( 19.08844512645451275, 183.3985617639965540, 309.1678998821465711 ) ) ;
#17770 = AXIS2_PLACEMENT_3D ( 'NONE', #7827, #11381, #13021 ) ;
#17771 = FACE_OUTER_BOUND ( 'NONE', #778, .T. ) ;
#17772 = AXIS2_PLACEMENT_3D ( 'NONE', #7762, #991, #6151 ) ;
#17773 = CARTESIAN_POINT ( 'NONE',  ( 91.14933227754937661, 79.20679280668171884, 26.78161688013026165 ) ) ;
#17774 = EDGE_CURVE ( 'NONE', #21224, #567, #15231, .T. ) ;
#17775 = DIRECTION ( 'NONE',  ( -0.9999164797902015955, 0.000000000000000000, 0.01292414190464174703 ) ) ;
#17776 = LINE ( 'NONE', #14787, #13624 ) ;
#17777 = VERTEX_POINT ( 'NONE', #13387 ) ;
#17778 = VECTOR ( 'NONE', #3688, 1000.000000000000000 ) ;
#17779 = AXIS2_PLACEMENT_3D ( 'NONE', #15415, #20207, #18714 ) ;
#17780 = CARTESIAN_POINT ( 'NONE',  ( -91.41775219751524162, 77.84255103198131565, -29.95431514105994353 ) ) ;
#17781 = ORIENTED_EDGE ( 'NONE', *, *, #5250, .T. ) ;
#17782 = B_SPLINE_CURVE_WITH_KNOTS ( 'NONE', 3,
 ( #19453, #7173, #1893, #52, #10739, #20828, #9107 ),
 .UNSPECIFIED., .F., .F.,
 ( 4, 3, 4 ),
 ( 0.000000000000000000, 2.978207829266235889E-05, 2.984123798783903494E-05 ),
 .UNSPECIFIED. ) ;
#17783 = AXIS2_PLACEMENT_3D ( 'NONE', #10425, #12272, #6960 ) ;
#17784 = VECTOR ( 'NONE', #1025, 1000.000000000000000 ) ;
#17785 = CARTESIAN_POINT ( 'NONE',  ( -69.49687660543771983, 70.17287388826144934, -85.26604680535984926 ) ) ;
#17786 = EDGE_CURVE ( 'NONE', #3794, #15416, #21616, .T. ) ;
#17787 = DIRECTION ( 'NONE',  ( 7.125109674161246868E-05, -0.9999848031710252272, 0.005512562950850154186 ) ) ;
#17788 = CARTESIAN_POINT ( 'NONE',  ( 161.9999999999998579, 0.000000000000000000, -10.00000000000224176 ) ) ;
#17789 = CARTESIAN_POINT ( 'NONE',  ( 44.31759907479521132, 171.6105373975396162, -53.08687767741515984 ) ) ;
#17790 = FACE_OUTER_BOUND ( 'NONE', #15462, .T. ) ;
#17791 = ORIENTED_EDGE ( 'NONE', *, *, #16987, .T. ) ;
#17792 = LINE ( 'NONE', #3863, #13571 ) ;
#17793 = VERTEX_POINT ( 'NONE', #4508 ) ;
#17794 = EDGE_LOOP ( 'NONE', ( #2193, #19397, #3624, #10998, #18904, #13168, #1851, #16928, #8167, #10564 ) ) ;
#17795 = VECTOR ( 'NONE', #13659, 1000.000000000000000 ) ;
#17796 = DIRECTION ( 'NONE',  ( 0.6979091139780387865, -0.003898296230782336263, -0.7161757269782926816 ) ) ;
#17797 = DIRECTION ( 'NONE',  ( 0.9999164797902015955, 2.001050586450178695E-22, -0.01292414190464131335 ) ) ;
#17798 = CARTESIAN_POINT ( 'NONE',  ( 66.18268079339601684, 69.99999999999998579, -87.86269266872859873 ) ) ;
#17799 = DIRECTION ( 'NONE',  ( 0.4910069343201003411, -0.004767316193522950878, -0.8711426192914037969 ) ) ;
#17800 = CARTESIAN_POINT ( 'NONE',  ( -88.44788333809836445, 80.14655074237849419, 31.99095626761631195 ) ) ;
#17801 = FACE_OUTER_BOUND ( 'NONE', #9090, .T. ) ;
#17802 = AXIS2_PLACEMENT_3D ( 'NONE', #22312, #16976, #4750 ) ;
#17803 = ORIENTED_EDGE ( 'NONE', *, *, #10203, .T. ) ;
#17804 = ADVANCED_FACE ( 'NONE', ( #16941 ), #6604, .F. ) ;
#17805 = CARTESIAN_POINT ( 'NONE',  ( -13.88059897197513060, 182.5799557881418593, 310.4051692506089921 ) ) ;
#17806 = AXIS2_PLACEMENT_3D ( 'NONE', #21387, #3832, #12456 ) ;
#17807 = ADVANCED_FACE ( 'NONE', ( #8302 ), #15335, .T. ) ;
#17808 = CARTESIAN_POINT ( 'NONE',  ( -58.84871535152515065, 114.6403824866543175, 163.0520739249805899 ) ) ;
#17809 = CARTESIAN_POINT ( 'NONE',  ( -39.75021781620441885, 72.00000000000000000, -86.03367798009510636 ) ) ;
#17810 = CARTESIAN_POINT ( 'NONE',  ( -14.96620062107659876, 178.7509044520041357, 316.1111495142839658 ) ) ;
#17811 =( REPRESENTATION_RELATIONSHIP ('NONE','NONE', #11808, #16508 ) REPRESENTATION_RELATIONSHIP_WITH_TRANSFORMATION ( #7214 )SHAPE_REPRESENTATION_RELATIONSHIP( ) );
#17812 = CARTESIAN_POINT ( 'NONE',  ( 20.64603878514330404, 181.9656304078110338, 315.4952833946043143 ) ) ;
#17813 = COLOUR_RGB ( '', 0.31764706, 0.68627451, 0.89019608) ;
#17814 = CARTESIAN_POINT ( 'NONE',  ( -41.42933370387425640, 166.0845032052916963, 276.3830402485593254 ) ) ;
#17815 = EDGE_CURVE ( 'NONE', #8361, #6866, #18543, .T. ) ;
#17816 = ITEM_DEFINED_TRANSFORMATION ( 'NONE', 'NONE', #18012,  #6292 ) ;
#17817 = PLANE ( 'NONE',  #12960 ) ;
#17818 = EDGE_CURVE ( 'NONE', #7542, #5831, #3130, .T. ) ;
#17819 = DIRECTION ( 'NONE',  ( 0.9999164797902017066, 4.653667080246435885E-16, -0.01292414190464085018 ) ) ;
#17820 = CARTESIAN_POINT ( 'NONE',  ( 50.14582690138693977, 111.1418060336978186, -47.81946391486589931 ) ) ;
#17821 = ORIENTED_EDGE ( 'NONE', *, *, #569, .T. ) ;
#17822 = VERTEX_POINT ( 'NONE', #1206 ) ;
#17823 = DIRECTION ( 'NONE',  ( 0.9506032891036972909, -0.3102281881984320644, -0.01057629388542894074 ) ) ;
#17824 = DIRECTION ( 'NONE',  ( -1.387778780781445044E-14, 0.000000000000000000, 1.000000000000000000 ) ) ;
#17825 = VERTEX_POINT ( 'NONE', #9916 ) ;
#17826 = CARTESIAN_POINT ( 'NONE',  ( 41.56623493000984126, 69.99999999999998579, 82.46967996629570052 ) ) ;
#17827 = EDGE_LOOP ( 'NONE', ( #16011, #1919, #7579, #9746 ) ) ;
#17828 = CARTESIAN_POINT ( 'NONE',  ( -59.95575053096360563, 114.2084250825692209, 165.7205294013835157 ) ) ;
#17829 = PLANE ( 'NONE',  #10814 ) ;
#17830 = VECTOR ( 'NONE', #7006, 1000.000000000000114 ) ;
#17831 = DIRECTION ( 'NONE',  ( -0.000000000000000000, -1.000000000000000000, -0.000000000000000000 ) ) ;
#17832 = FACE_OUTER_BOUND ( 'NONE', #1096, .T. ) ;
#17833 = ADVANCED_FACE ( 'NONE', ( #6578 ), #4722, .F. ) ;
#17834 = VERTEX_POINT ( 'NONE', #20582 ) ;
#17835 = VERTEX_POINT ( 'NONE', #1425 ) ;
#17836 = CARTESIAN_POINT ( 'NONE',  ( 9.722607335555387920, 142.9425743169972520, 274.9463719921606071 ) ) ;
#17837 = LINE ( 'NONE', #9053, #9895 ) ;
#17838 = VERTEX_POINT ( 'NONE', #22186 ) ;
#17839 = B_SPLINE_CURVE_WITH_KNOTS ( 'NONE', 3,
 ( #14468, #8788, #21433, #14114, #21529, #10536, #3961, #548, #19366, #14228, #5348, #9138, #17555, #1803 ),
 .UNSPECIFIED., .F., .F.,
 ( 4, 2, 2, 2, 2, 2, 4 ),
 ( 0.000000000000000000, 0.0003918831267809858715, 0.0007837662535619717430, 0.001175649380342957831, 0.001567532507123943486, 0.002351298760685859284, 0.003135065014247775082 ),
 .UNSPECIFIED. ) ;
#17840 = DIRECTION ( 'NONE',  ( -0.9999164797902015955, 8.863511990578707937E-16, 0.01292414190464158050 ) ) ;
#17841 = CARTESIAN_POINT ( 'NONE',  ( -89.92684002299503732, 87.84535921386273571, 50.88169406451069676 ) ) ;
#17842 = SHAPE_DEFINITION_REPRESENTATION ( #11206, #5468 ) ;
#17843 = CIRCLE ( 'NONE', #4228, 2.000000000000004441 ) ;
#17845 = ORIENTED_EDGE ( 'NONE', *, *, #1069, .F. ) ;
#17844 = ORIENTED_EDGE ( 'NONE', *, *, #22241, .T. ) ;
#17846 = EDGE_CURVE ( 'NONE', #7720, #19552, #21993, .T. ) ;
#17847 = ORIENTED_EDGE ( 'NONE', *, *, #12663, .F. ) ;
#17848 = DIRECTION ( 'NONE',  ( -1.372099599554306628E-14, 0.000000000000000000, 1.000000000000000000 ) ) ;
#17849 = DIRECTION ( 'NONE',  ( -2.025474946048326158E-22, 1.000000000000000000, -1.876735158486678933E-22 ) ) ;
#17850 = ORIENTED_EDGE ( 'NONE', *, *, #78, .F. ) ;
#17851 = CARTESIAN_POINT ( 'NONE',  ( -105.6848962833589383, 69.99999999999998579, -30.50771805806158454 ) ) ;
#17852 = LINE ( 'NONE', #8969, #7094 ) ;
#17853 = ORIENTED_EDGE ( 'NONE', *, *, #13702, .T. ) ;
#17854 = CARTESIAN_POINT ( 'NONE',  ( 91.44886093103751534, 77.80125034018027463, 29.89077835665231930 ) ) ;
#17855 = ORIENTED_EDGE ( 'NONE', *, *, #13702, .F. ) ;
#17856 = CARTESIAN_POINT ( 'NONE',  ( -61.06315242452672010, 118.9229714579762742, 168.3606140555295951 ) ) ;
#17857 = CARTESIAN_POINT ( 'NONE',  ( -59.21355730958399732, 118.5884715842524173, 107.6580735039648431 ) ) ;
#17858 = DIRECTION ( 'NONE',  ( 0.01292394549866739996, 0.005513023399721131770, 0.9999012842304692006 ) ) ;
#17859 = CARTESIAN_POINT ( 'NONE',  ( -10.83342074598470184, 165.0533908189748900, 320.2543728156808243 ) ) ;
#17860 = CARTESIAN_POINT ( 'NONE',  ( -105.9973908263409328, 79.15210294646404066, 29.40494008559752714 ) ) ;
#17861 = ADVANCED_FACE ( 'NONE', ( #8404 ), #15448, .F. ) ;
#17862 = EDGE_LOOP ( 'NONE', ( #8890, #5487, #4327, #4478 ) ) ;
#17863 = CARTESIAN_POINT ( 'NONE',  ( -39.85606267361366406, 107.1132303434984578, 71.72685069023916071 ) ) ;
#17864 = DIRECTION ( 'NONE',  ( 0.4397038457472424167, 0.000000000000000000, -0.8981428216242032248 ) ) ;
#17865 = AXIS2_PLACEMENT_3D ( 'NONE', #17469, #3317, #21005 ) ;
#17866 = CARTESIAN_POINT ( 'NONE',  ( -37.54386652542168434, 92.77591188308413450, -82.72434418715882032 ) ) ;
#17867 = VERTEX_POINT ( 'NONE', #971 ) ;
#17868 = DIRECTION ( 'NONE',  ( -0.01292394549866632963, -0.005513023399716958026, -0.9999012842304692006 ) ) ;
#17869 = VERTEX_POINT ( 'NONE', #20674 ) ;
#17870 = ORIENTED_EDGE ( 'NONE', *, *, #11734, .T. ) ;
#17871 = PLANE ( 'NONE',  #2368 ) ;
#17872 = ORIENTED_EDGE ( 'NONE', *, *, #1387, .F. ) ;
#17873 = EDGE_CURVE ( 'NONE', #9660, #13237, #8082, .T. ) ;
#17874 = CARTESIAN_POINT ( 'NONE',  ( 49.39887009976201426, 113.4706157781613598, -46.83140348491149041 ) ) ;
#17875 = ADVANCED_FACE ( 'NONE', ( #3106 ), #2932, .T. ) ;
#17876 = DIRECTION ( 'NONE',  ( 0.9999164797902017066, 0.000000000000000000, -0.01292414190464177826 ) ) ;
#17877 = CARTESIAN_POINT ( 'NONE',  ( -1.163172771417702478, 95.03750572909316929, -89.99248318111824574 ) ) ;
#17878 = CARTESIAN_POINT ( 'NONE',  ( -91.38403781951991789, 79.16811561863683266, -26.65243986599113768 ) ) ;
#17879 = CARTESIAN_POINT ( 'NONE',  ( -40.09630628311408884, 94.23964578315411700, 84.16448747414683851 ) ) ;
#17880 = VECTOR ( 'NONE', #10224, 1000.000000000000000 ) ;
#17881 = CARTESIAN_POINT ( 'NONE',  ( -64.10659645996310019, 93.47724784606892001, 69.54099877995811596 ) ) ;
#17882 = CARTESIAN_POINT ( 'NONE',  ( 74.64244246480362222, 75.05735400057622542, -4.269988455633038527 ) ) ;
#17883 = CARTESIAN_POINT ( 'NONE',  ( 12.31508922632070302, 187.5663303611497383, 304.9177876444722983 ) ) ;
#17884 = CARTESIAN_POINT ( 'NONE',  ( 91.32446103601381537, 78.00118640252709667, 30.19495016275310917 ) ) ;
#17885 = CARTESIAN_POINT ( 'NONE',  ( 92.11907261954644355, 79.08352528315391794, 26.36518256425470241 ) ) ;
#17886 = DIRECTION ( 'NONE',  ( -0.01292394549866741384, -0.005513023399720269613, -0.9999012842304692006 ) ) ;
#17887 = DIRECTION ( 'NONE',  ( 2.025474946048326158E-22, -1.000000000000000000, 1.876735158486679638E-22 ) ) ;
#17888 = ORIENTED_EDGE ( 'NONE', *, *, #452, .F. ) ;
#17889 = CARTESIAN_POINT ( 'NONE',  ( -34.79755969384669356, 125.3640259171584290, 248.0123345355920890 ) ) ;
#17890 = ORIENTED_EDGE ( 'NONE', *, *, #10512, .F. ) ;
#17891 = VECTOR ( 'NONE', #11718, 1000.000000000000114 ) ;
#17892 = B_SPLINE_CURVE_WITH_KNOTS ( 'NONE', 3,
 ( #20189, #6434, #13444, #1378, #20412, #4671, #11704, #18699, #2969, #9985, #13547, #8352, #20527, #4459, #17012, #8261, #20653, #11832 ),
 .UNSPECIFIED., .F., .F.,
 ( 4, 2, 2, 2, 2, 2, 2, 2, 4 ),
 ( 0.000000000000000000, 0.1250000000000000000, 0.2500000000000000000, 0.3750000000000000000, 0.5000000000000000000, 0.6250000000000000000, 0.7500000000000000000, 0.8750000000000000000, 1.000000000000000000 ),
 .UNSPECIFIED. ) ;
#17893 = LINE ( 'NONE', #9126, #8803 ) ;
#17894 = CARTESIAN_POINT ( 'NONE',  ( -6.847138702882150874, 173.1019677278035829, 81.67819396028960455 ) ) ;
#17895 = FACE_OUTER_BOUND ( 'NONE', #6761, .T. ) ;
#17896 = CARTESIAN_POINT ( 'NONE',  ( -110.8973471360828285, 103.0000000000000000, -68.71519772349600430 ) ) ;
#17897 = CYLINDRICAL_SURFACE ( 'NONE', #14820, 6.499999999999998224 ) ;
#17898 = ORIENTED_EDGE ( 'NONE', *, *, #15011, .T. ) ;
#17899 = DIRECTION ( 'NONE',  ( -0.01292394549866745720, -0.005513023399720816918, -0.9999012842304692006 ) ) ;
#17900 = ORIENTED_EDGE ( 'NONE', *, *, #3919, .T. ) ;
#17901 = ORIENTED_EDGE ( 'NONE', *, *, #9779, .F. ) ;
#17902 = DIRECTION ( 'NONE',  ( -0.009760756503428008254, 0.9999378516499564107, -0.005387065077611006073 ) ) ;
#17903 = AXIS2_PLACEMENT_3D ( 'NONE', #7937, #14632, #715 ) ;
#17904 = FACE_OUTER_BOUND ( 'NONE', #20136, .T. ) ;
#17905 = PLANE ( 'NONE',  #11095 ) ;
#17906 = CARTESIAN_POINT ( 'NONE',  ( -88.82392706003518867, 79.74373590868249551, 30.79623470077038050 ) ) ;
#17907 = FACE_OUTER_BOUND ( 'NONE', #8747, .T. ) ;
#17908 = VERTEX_POINT ( 'NONE', #20439 ) ;
#17909 = DIRECTION ( 'NONE',  ( 1.387778780781444571E-14, 0.000000000000000000, -1.000000000000000000 ) ) ;
#17910 = B_SPLINE_CURVE_WITH_KNOTS ( 'NONE', 3,
 ( #16246, #9321, #836, #7595, #4360, #16466, #14752, #11277, #18074, #14631, #17959, #10936, #11386, #3915, #9551, #371 ),
 .UNSPECIFIED., .F., .F.,
 ( 4, 2, 2, 2, 2, 2, 2, 4 ),
 ( 0.000000000000000000, 0.0008607555596716879491, 0.001291133339507522654, 0.001721511119343357467, 0.002151888899179192280, 0.002582266679015027093, 0.003012644458850861906, 0.003443022238686696719 ),
 .UNSPECIFIED. ) ;
#17911 = ORIENTED_EDGE ( 'NONE', *, *, #20592, .F. ) ;
#17912 = FACE_OUTER_BOUND ( 'NONE', #10120, .T. ) ;
#17913 = DIRECTION ( 'NONE',  ( 0.4540042784513456109, 0.000000000000000000, -0.8909995034498464639 ) ) ;
#17914 = CARTESIAN_POINT ( 'NONE',  ( -14.48496598153953485, 181.1498399189628969, 317.9007409887333893 ) ) ;
#17915 = EDGE_LOOP ( 'NONE', ( #9042, #15894 ) ) ;
#17916 = DIRECTION ( 'NONE',  ( -0.01292394549866754394, -0.005513023399720772683, -0.9999012842304692006 ) ) ;
#17917 = EDGE_LOOP ( 'NONE', ( #20546, #14738, #21859, #5455 ) ) ;
#17918 = AXIS2_PLACEMENT_3D ( 'NONE', #14968, #11168, #2547 ) ;
#17919 = CARTESIAN_POINT ( 'NONE',  ( 1.117803423002105445, 55.00000000000000000, 109.6947150755565161 ) ) ;
#17920 = AXIS2_PLACEMENT_3D ( 'NONE', #11641, #10031, #18637 ) ;
#17921 = ADVANCED_FACE ( 'NONE', ( #15082 ), #8281, .F. ) ;
#17922 = CARTESIAN_POINT ( 'NONE',  ( -35.37437755136378570, 92.78536193180231351, 83.65759506009349877 ) ) ;
#17923 = DIRECTION ( 'NONE',  ( 0.3102455404053300891, 0.9506564598521406451, 0.000000000000000000 ) ) ;
#17924 = CARTESIAN_POINT ( 'NONE',  ( 50.65705442791912816, 111.6851564030456103, -48.02593606187189579 ) ) ;
#17925 = AXIS2_PLACEMENT_3D ( 'NONE', #7896, #19996, #16373 ) ;
#17926 = ORIENTED_EDGE ( 'NONE', *, *, #3883, .T. ) ;
#17927 = DIRECTION ( 'NONE',  ( 7.125109674403850657E-05, -0.9999848031710253382, 0.005512562950847868688 ) ) ;
#17928 = CARTESIAN_POINT ( 'NONE',  ( 51.42455095033977130, 113.4816418249608034, -44.85744920025983618 ) ) ;
#17929 = ORIENTED_EDGE ( 'NONE', *, *, #3822, .F. ) ;
#17930 = FACE_OUTER_BOUND ( 'NONE', #21131, .T. ) ;
#17931 = CARTESIAN_POINT ( 'NONE',  ( 0.000000000000000000, 45.00000000000000000, 0.000000000000000000 ) ) ;
#17932 = CARTESIAN_POINT ( 'NONE',  ( 153.9999999999992610, 20.00000000000000000, -53.76161406891471017 ) ) ;
#17933 = DIRECTION ( 'NONE',  ( 0.9934404589540162256, 0.1135548637187060589, -0.01346653032743021922 ) ) ;
#17934 = EDGE_CURVE ( 'NONE', #15373, #13257, #11727, .T. ) ;
#17935 = ORIENTED_EDGE ( 'NONE', *, *, #15837, .F. ) ;
#17936 = CARTESIAN_POINT ( 'NONE',  ( 20.70083805927512088, 149.3646325075532957, 278.4026507072620120 ) ) ;
#17937 = CARTESIAN_POINT ( 'NONE',  ( -2.322807172541347498, 81.99999999999998579, -81.06750429846923112 ) ) ;
#17938 = EDGE_CURVE ( 'NONE', #168, #8602, #16800, .T. ) ;
#17939 = ORIENTED_EDGE ( 'NONE', *, *, #22361, .T. ) ;
#17940 = CARTESIAN_POINT ( 'NONE',  ( 42.02709154643847000, 106.9581013127162379, 70.53115534494513383 ) ) ;
#17941 = CARTESIAN_POINT ( 'NONE',  ( -90.09632239900712136, 87.49413173051891590, 51.09744761898891596 ) ) ;
#17942 = VECTOR ( 'NONE', #16611, 999.9999999999998863 ) ;
#17943 = APPLICATION_PROTOCOL_DEFINITION ( 'draft international standard', 'automotive_design', 1998, #2661 ) ;
#17944 = VECTOR ( 'NONE', #12025, 1000.000000000000000 ) ;
#17945 = EDGE_CURVE ( 'NONE', #7906, #10199, #13693, .T. ) ;
#17946 = EDGE_LOOP ( 'NONE', ( #5008, #20091, #9669, #15698, #9594 ) ) ;
#17947 = EDGE_CURVE ( 'NONE', #5612, #7136, #15314, .T. ) ;
#17948 = VERTEX_POINT ( 'NONE', #22484 ) ;
#17949 = DIRECTION ( 'NONE',  ( -0.009188991635466048358, 0.7031977391749438810, -0.7109349492407661675 ) ) ;
#17950 = EDGE_CURVE ( 'NONE', #5625, #18285, #6456, .T. ) ;
#17951 = DIRECTION ( 'NONE',  ( 0.9999164797902017066, 0.000000000000000000, -0.01292414190464177826 ) ) ;
#17952 = EDGE_CURVE ( 'NONE', #11828, #16423, #2990, .T. ) ;
#17953 = PLANE ( 'NONE',  #11593 ) ;
#17954 = CYLINDRICAL_SURFACE ( 'NONE', #17770, 7.499999999999992006 ) ;
#17955 = ORIENTED_EDGE ( 'NONE', *, *, #22241, .F. ) ;
#17956 = CARTESIAN_POINT ( 'NONE',  ( 47.42620204064805023, 94.99786382055523859, -44.70385809434849733 ) ) ;
#17957 = ORIENTED_EDGE ( 'NONE', *, *, #12368, .F. ) ;
#17958 = DIRECTION ( 'NONE',  ( -0.3834992599886433706, 0.005063754594578209756, 0.9235273011544211652 ) ) ;
#17959 = CARTESIAN_POINT ( 'NONE',  ( -92.25563491934029514, 77.27426140725017945, -29.04871113840125219 ) ) ;
#17960 = CARTESIAN_POINT ( 'NONE',  ( -78.25644772108614688, 75.12006735377332234, -3.764112139945209989 ) ) ;
#17961 = CARTESIAN_POINT ( 'NONE',  ( -13.55891735653775676, 164.7118933236453415, 312.8669722336247219 ) ) ;
#17962 = AXIS2_PLACEMENT_3D ( 'NONE', #7334, #14380, #21231 ) ;
#17963 = DIRECTION ( 'NONE',  ( 0.01125613334114018010, 0.4913919529878011949, 0.8708658036695671179 ) ) ;
#17964 = ORIENTED_EDGE ( 'NONE', *, *, #18029, .T. ) ;
#17965 = CARTESIAN_POINT ( 'NONE',  ( 1.143879619237349266, 165.4878736975560969, 88.49980839044366121 ) ) ;
#17966 = DIRECTION ( 'NONE',  ( 2.449293598294706414E-16, 0.000000000000000000, 1.000000000000000000 ) ) ;
#17967 = CIRCLE ( 'NONE', #18674, 4.500000000000006217 ) ;
#17968 = CARTESIAN_POINT ( 'NONE',  ( -52.22280431992486882, 111.8670818006853551, -46.76325931430218219 ) ) ;
#17969 = VERTEX_POINT ( 'NONE', #10009 ) ;
#17970 = CARTESIAN_POINT ( 'NONE',  ( -55.33804461215960657, 114.2193244133317904, 167.6379947637574617 ) ) ;
#17971 = ADVANCED_FACE ( 'NONE', ( #12073, #4932 ), #17238, .F. ) ;
#17972 = EDGE_LOOP ( 'NONE', ( #7637, #21669, #4364, #18437, #8606 ) ) ;
#17973 = CARTESIAN_POINT ( 'NONE',  ( 86.79222083800954124, 104.3814432989690602, 67.58039954014910222 ) ) ;
#17974 = ORIENTED_EDGE ( 'NONE', *, *, #13250, .T. ) ;
#17975 = CIRCLE ( 'NONE', #16148, 10.99999999999999822 ) ;
#17977 = ORIENTED_EDGE ( 'NONE', *, *, #19452, .F. ) ;
#17976 = EDGE_LOOP ( 'NONE', ( #7730, #22455, #10137, #4547 ) ) ;
#17978 = COLOUR_RGB ( '', 0.40784314, 0.44705882, 0.49803922) ;
#17979 = EDGE_CURVE ( 'NONE', #1849, #13913, #13653, .T. ) ;
#17980 = VECTOR ( 'NONE', #18166, 1000.000000000000227 ) ;
#17981 = CARTESIAN_POINT ( 'NONE',  ( 5.047586898063077143, 159.3382231987902173, 324.6243296352952825 ) ) ;
#17982 = DIRECTION ( 'NONE',  ( -0.9934404589540162256, -0.1135548637187056842, 0.01346653032743081423 ) ) ;
#17983 = CARTESIAN_POINT ( 'NONE',  ( 5.149300590115022835, 70.80384757729338219, -98.24794683011701579 ) ) ;
#17984 = DIRECTION ( 'NONE',  ( 0.01292394549866738608, 0.005513023399720699824, 0.9999012842304692006 ) ) ;
#17985 = LINE ( 'NONE', #14778, #8780 ) ;
#17986 = CARTESIAN_POINT ( 'NONE',  ( 16.77746333736591566, 186.8979171237260459, 277.5925732922278257 ) ) ;
#17987 = CARTESIAN_POINT ( 'NONE',  ( 14.87756490533177356, 186.3606781135739823, 305.6069114145042818 ) ) ;
#17988 = CARTESIAN_POINT ( 'NONE',  ( 89.98285967923904138, 79.53265832318567163, 27.83436926225109431 ) ) ;
#17989 = CARTESIAN_POINT ( 'NONE',  ( 90.71810225913510806, 79.29666913609152346, 27.07744225877261712 ) ) ;
#17990 = CIRCLE ( 'NONE', #750, 3.999999999999995559 ) ;
#17991 = EDGE_CURVE ( 'NONE', #2134, #1879, #10355, .T. ) ;
#17992 = DIRECTION ( 'NONE',  ( 7.125109674364536131E-05, -0.9999848031710253382, 0.005512562950849705760 ) ) ;
#17993 = LINE ( 'NONE', #1903, #17294 ) ;
#17994 = EDGE_CURVE ( 'NONE', #9131, #9564, #2279, .T. ) ;
#17995 = AXIS2_PLACEMENT_3D ( 'NONE', #21769, #16204, #14482 ) ;
#17996 = ORIENTED_EDGE ( 'NONE', *, *, #19593, .T. ) ;
#17997 = CARTESIAN_POINT ( 'NONE',  ( -92.80269534486276939, 79.83421200779902449, -28.82571798309893651 ) ) ;
#17998 = ORIENTED_EDGE ( 'NONE', *, *, #2591, .T. ) ;
#17999 = CARTESIAN_POINT ( 'NONE',  ( -1.446236478174512063, 70.01899995639453778, -80.95361029988728774 ) ) ;
#18000 = AXIS2_PLACEMENT_3D ( 'NONE', #4207, #5935, #20391 ) ;
#18001 = CARTESIAN_POINT ( 'NONE',  ( 11.52330416447161276, 174.5538381589252594, 299.4542690950677297 ) ) ;
#18002 = FILL_AREA_STYLE ('',( #1914 ) ) ;
#18003 = CARTESIAN_POINT ( 'NONE',  ( 19.14437128616974348, 137.4882992087673870, 88.42152559878388729 ) ) ;
#18004 = AXIS2_PLACEMENT_3D ( 'NONE', #3261, #17302, #1562 ) ;
#18005 = CARTESIAN_POINT ( 'NONE',  ( -55.37247063347942344, 143.9050905090121546, 164.9745184335410784 ) ) ;
#18006 = CARTESIAN_POINT ( 'NONE',  ( 80.48140932536705350, 75.20583697296392245, 5.210614517255996780 ) ) ;
#18007 = AXIS2_PLACEMENT_3D ( 'NONE', #6694, #4955, #11987 ) ;
#18008 = LINE ( 'NONE', #16182, #2700 ) ;
#18009 = ORIENTED_EDGE ( 'NONE', *, *, #20695, .T. ) ;
#18010 = LINE ( 'NONE', #10874, #21956 ) ;
#18011 = DIRECTION ( 'NONE',  ( -0.02821419319640158449, -4.204905210891534595E-06, 0.9996019004006518882 ) ) ;
#18012 = AXIS2_PLACEMENT_3D ( 'NONE', #21794, #3901, #10923 ) ;
#18013 = CARTESIAN_POINT ( 'NONE',  ( -55.50260078534234509, 114.1916338672434534, 162.6170270725387468 ) ) ;
#18014 = DIRECTION ( 'NONE',  ( 0.01292414190464174703, 0.000000000000000000, 0.9999164797902015955 ) ) ;
#18015 = VECTOR ( 'NONE', #20955, 1000.000000000000000 ) ;
#18016 = CARTESIAN_POINT ( 'NONE',  ( -89.40066202591053468, 79.46807343419025926, 29.95041408109006653 ) ) ;
#18017 = CARTESIAN_POINT ( 'NONE',  ( -62.57984418954151806, 127.0293918815981442, 187.6629419631760243 ) ) ;
#18018 = VERTEX_POINT ( 'NONE', #3204 ) ;
#18019 = CARTESIAN_POINT ( 'NONE',  ( -39.39497909003006981, 72.00000000000000000, 85.51628863845817818 ) ) ;
#18020 = ORIENTED_EDGE ( 'NONE', *, *, #6669, .T. ) ;
#18021 = EDGE_CURVE ( 'NONE', #3219, #12722, #8486, .T. ) ;
#18022 = CARTESIAN_POINT ( 'NONE',  ( -90.41042953090172318, 78.34730160488616946, 33.05240787946384984 ) ) ;
#18023 = CARTESIAN_POINT ( 'NONE',  ( -15.53263949983598202, 177.8010796364676480, 313.8283261121160876 ) ) ;
#18024 = VERTEX_POINT ( 'NONE', #8379 ) ;
#18025 = CIRCLE ( 'NONE', #8098, 9.000000000000001776 ) ;
#18026 = ORIENTED_EDGE ( 'NONE', *, *, #632, .T. ) ;
#18027 = VECTOR ( 'NONE', #15600, 1000.000000000000227 ) ;
#18028 = CARTESIAN_POINT ( 'NONE',  ( 105.4334892372614405, 77.12912189496645965, -31.36525700924962834 ) ) ;
#18029 = EDGE_CURVE ( 'NONE', #8567, #13491, #17129, .T. ) ;
#18030 = ORIENTED_EDGE ( 'NONE', *, *, #11755, .F. ) ;
#18031 = CARTESIAN_POINT ( 'NONE',  ( -34.79044227946425849, 119.3672327899910073, 248.5629954604718534 ) ) ;
#18032 = AXIS2_PLACEMENT_3D ( 'NONE', #8210, #20368, #9925 ) ;
#18033 = PRODUCT_RELATED_PRODUCT_CATEGORY ( 'part', '', ( #15071 ) ) ;
#18034 = DIRECTION ( 'NONE',  ( 0.01292394549866731149, 0.005513023399720593139, 0.9999012842304692006 ) ) ;
#18035 = DIRECTION ( 'NONE',  ( 0.7116070947332637786, 0.08419371040299428177, 0.6975147036829121294 ) ) ;
#18036 = EDGE_LOOP ( 'NONE', ( #15781, #16441, #4781, #5573, #3697 ) ) ;
#18037 = CARTESIAN_POINT ( 'NONE',  ( 64.99457118636310327, 170.0000000000000284, -0.8400692238017243296 ) ) ;
#18038 = VECTOR ( 'NONE', #17887, 1000.000000000000000 ) ;
#18039 = EDGE_LOOP ( 'NONE', ( #1470, #14287, #11855, #14905 ) ) ;
#18040 = DIRECTION ( 'NONE',  ( 0.009088227368120579963, 0.7109943316365083810, 0.7031390079522398251 ) ) ;
#18041 = ORIENTED_EDGE ( 'NONE', *, *, #8691, .F. ) ;
#18042 = ORIENTED_EDGE ( 'NONE', *, *, #7097, .F. ) ;
#18043 = CARTESIAN_POINT ( 'NONE',  ( -14.85278902669711520, 137.4882992087673870, 88.86094642354169082 ) ) ;
#18044 = FACE_OUTER_BOUND ( 'NONE', #3734, .T. ) ;
#18045 = CARTESIAN_POINT ( 'NONE',  ( -40.54068192821626582, 96.15465585523027414, -41.57304724140053764 ) ) ;
#18046 = PLANE ( 'NONE',  #12197 ) ;
#18047 = ORIENTED_EDGE ( 'NONE', *, *, #11609, .F. ) ;
#18048 = DIRECTION ( 'NONE',  ( 0.9999164797902015955, 6.965998958219364448E-18, -0.01292414190464157182 ) ) ;
#18049 = AXIS2_PLACEMENT_3D ( 'NONE', #10314, #92, #19028 ) ;
#18050 = EDGE_CURVE ( 'NONE', #22002, #8399, #15531, .T. ) ;
#18051 = CARTESIAN_POINT ( 'NONE',  ( -0.8801090646609045498, 81.98100004360541959, -99.03135606234927479 ) ) ;
#18052 = ORIENTED_EDGE ( 'NONE', *, *, #5168, .T. ) ;
#18053 = CIRCLE ( 'NONE', #15500, 2.000000000000002665 ) ;
#18054 = DIRECTION ( 'NONE',  ( 7.125109674364534776E-05, -0.9999848031710252272, 0.005512562950849704893 ) ) ;
#18055 = AXIS2_PLACEMENT_3D ( 'NONE', #1060, #6673, #20559 ) ;
#18056 = CARTESIAN_POINT ( 'NONE',  ( -88.18034797016093762, 89.00358945086300366, 51.18297751363882497 ) ) ;
#18057 =( GEOMETRIC_REPRESENTATION_CONTEXT ( 3 ) GLOBAL_UNCERTAINTY_ASSIGNED_CONTEXT ( ( #6316 ) ) GLOBAL_UNIT_ASSIGNED_CONTEXT ( ( #10965, #11422, #6025 ) ) REPRESENTATION_CONTEXT ( 'NONE', 'WORKASPACE' ) );
#18058 =( NAMED_UNIT ( * ) PLANE_ANGLE_UNIT ( ) SI_UNIT ( $, .RADIAN. ) );
#18059 = AXIS2_PLACEMENT_3D ( 'NONE', #20537, #4680, #1164 ) ;
#18060 = ORIENTED_EDGE ( 'NONE', *, *, #13973, .T. ) ;
#18061 = ADVANCED_FACE ( 'NONE', ( #20550, #9889, #16913, #1179 ), #11853, .F. ) ;
#18062 = FACE_OUTER_BOUND ( 'NONE', #22587, .T. ) ;
#18063 = ORIENTED_EDGE ( 'NONE', *, *, #18757, .F. ) ;
#18064 = DIRECTION ( 'NONE',  ( 0.01292394549866728373, 0.005513023399720296501, 0.9999012842304693116 ) ) ;
#18065 = VECTOR ( 'NONE', #6791, 1000.000000000000000 ) ;
#18066 = CARTESIAN_POINT ( 'NONE',  ( 1.054933926688728762, 165.4499317482979279, 81.61824794009152129 ) ) ;
#18067 = CARTESIAN_POINT ( 'NONE',  ( 65.91440269377942229, 103.0000000000000000, 70.32555938675403695 ) ) ;
#18068 = CARTESIAN_POINT ( 'NONE',  ( 396.9612392269590373, 103.0000000000000000, 66.04670572356099001 ) ) ;
#18069 = ORIENTED_EDGE ( 'NONE', *, *, #19692, .F. ) ;
#18070 = EDGE_CURVE ( 'NONE', #22032, #13714, #2644, .T. ) ;
#18071 = CARTESIAN_POINT ( 'NONE',  ( 92.25563491934033777, 77.27426140725016523, 29.04871113840120600 ) ) ;
#18072 = ORIENTED_EDGE ( 'NONE', *, *, #5269, .T. ) ;
#18073 = CARTESIAN_POINT ( 'NONE',  ( -54.68979215835705077, 114.2467007792763098, 172.5957179600166569 ) ) ;
#18074 = CARTESIAN_POINT ( 'NONE',  ( -91.92156639752093383, 77.41735670888594711, -29.28407961425102002 ) ) ;
#18075 = CARTESIAN_POINT ( 'NONE',  ( -13.54442673061105573, 147.0068218323744134, 276.9278867193614246 ) ) ;
#18076 = DIRECTION ( 'NONE',  ( -0.01292394549866739996, -0.005513023399721131770, -0.9999012842304692006 ) ) ;
#18077 = CONICAL_SURFACE ( 'NONE', #6343, 9.000000000000001776, 1.047197551196594301 ) ;
#18078 = VECTOR ( 'NONE', #22137, 999.9999999999998863 ) ;
#18079 = AXIS2_PLACEMENT_3D ( 'NONE', #2386, #2488, #896 ) ;
#18080 = CARTESIAN_POINT ( 'NONE',  ( -39.06289137140529988, 108.3156947416822362, 72.76082051835628306 ) ) ;
#18081 = CARTESIAN_POINT ( 'NONE',  ( -55.33808647217894361, 114.8068154851947753, 167.6347561330238420 ) ) ;
#18082 = CARTESIAN_POINT ( 'NONE',  ( -162.0000000000000000, 20.00000000000000000, 3.967855629237424480E-14 ) ) ;
#18083 = CARTESIAN_POINT ( 'NONE',  ( 40.27217859821899282, 105.8205586461024552, 91.88447881881737089 ) ) ;
#18084 = EDGE_CURVE ( 'NONE', #12773, #20154, #1066, .T. ) ;
#18085 = EDGE_LOOP ( 'NONE', ( #16067, #9096, #6789, #2312, #11850, #6373, #7467, #7988 ) ) ;
#18086 = CARTESIAN_POINT ( 'NONE',  ( 12.81503532323078964, 190.4972571607467842, 307.8483445055002221 ) ) ;
#18087 = EDGE_CURVE ( 'NONE', #21893, #6852, #14010, .T. ) ;
#18088 = VECTOR ( 'NONE', #4584, 1000.000000000000000 ) ;
#18089 = EDGE_LOOP ( 'NONE', ( #6077, #4852 ) ) ;
#18090 = ORIENTED_EDGE ( 'NONE', *, *, #12588, .F. ) ;
#18091 = CARTESIAN_POINT ( 'NONE',  ( -83.88046665555830828, 75.05943625219151727, -2.284324781586978048 ) ) ;
#18092 = CARTESIAN_POINT ( 'NONE',  ( -90.14880203183271590, 88.11115007023326484, 53.04766197139571204 ) ) ;
#18093 = VECTOR ( 'NONE', #792, 999.9999999999998863 ) ;
#18094 = ORIENTED_EDGE ( 'NONE', *, *, #676, .T. ) ;
#18095 = VERTEX_POINT ( 'NONE', #10681 ) ;
#18096 = ADVANCED_FACE ( 'NONE', ( #122 ), #16103, .F. ) ;
#18097 = CARTESIAN_POINT ( 'NONE',  ( 3.833582208902202471, 166.6352317792378415, 296.5970240496424708 ) ) ;
#18098 = CARTESIAN_POINT ( 'NONE',  ( 58.90710753996705762, 143.6018742220277318, 108.4936714818314698 ) ) ;
#18099 = CARTESIAN_POINT ( 'NONE',  ( -53.22343177146392179, 169.4762627770265340, -94.31856662285323978 ) ) ;
#18100 = CARTESIAN_POINT ( 'NONE',  ( -37.17546262443868699, 94.47305566264986965, 83.89071743665799374 ) ) ;
#18101 = ADVANCED_FACE ( 'NONE', ( #17832 ), #6881, .F. ) ;
#18102 = AXIS2_PLACEMENT_3D ( 'NONE', #1136, #21775, #19949 ) ;
#18103 = CARTESIAN_POINT ( 'NONE',  ( 3.911668260932484209, 158.6357289660382719, 296.6401205702638322 ) ) ;
#18104 = CARTESIAN_POINT ( 'NONE',  ( 13.86180204460999299, 188.5620406374387414, 276.5865498250307155 ) ) ;
#18105 = CARTESIAN_POINT ( 'NONE',  ( 20.02685672050394317, 182.6349384657623887, 315.1934792567789714 ) ) ;
#18106 = CARTESIAN_POINT ( 'NONE',  ( 93.05058556066120445, 79.82257531472971834, 28.80218916741394253 ) ) ;
#18107 = B_SPLINE_CURVE_WITH_KNOTS ( 'NONE', 3,
 ( #3248, #13406, #22529, #20377, #13508, #15134, #3145, #11664, #6494, #9936, #20484, #16964, #1228, #10059, #10274, #17076 ),
 .UNSPECIFIED., .F., .F.,
 ( 4, 2, 2, 2, 2, 2, 2, 4 ),
 ( 1.962615573354718958E-17, 0.0003919156718472174578, 0.0007838313436944152916, 0.001175747015541613342, 0.001567662687388811068, 0.002351494031083169439, 0.002743409702930348516, 0.003135325374777527159 ),
 .UNSPECIFIED. ) ;
#18108 = CARTESIAN_POINT ( 'NONE',  ( 146.4999999999998579, 2.000000000000000000, -10.00000000000202682 ) ) ;
#18109 =( NAMED_UNIT ( * ) PLANE_ANGLE_UNIT ( ) SI_UNIT ( $, .RADIAN. ) );
#18110 = AXIS2_PLACEMENT_3D ( 'NONE', #12055, #14012, #6984 ) ;
#18111 = AXIS2_PLACEMENT_3D ( 'NONE', #8282, #11625, #13471 ) ;
#18112 = EDGE_CURVE ( 'NONE', #9516, #11382, #18772, .T. ) ;
#18113 = CARTESIAN_POINT ( 'NONE',  ( 3.833582208902202471, 166.6352317792378415, 296.5970240496424708 ) ) ;
#18114 = CARTESIAN_POINT ( 'NONE',  ( -1.124400345703781001, 72.00000000000000000, -86.99273374174757123 ) ) ;
#18115 = ORIENTED_EDGE ( 'NONE', *, *, #5912, .F. ) ;
#18116 = DIRECTION ( 'NONE',  ( -0.01292394549866733230, -0.005513023399720419666, -0.9999012842304692006 ) ) ;
#18117 = ORIENTED_EDGE ( 'NONE', *, *, #3480, .F. ) ;
#18118 = DIRECTION ( 'NONE',  ( 0.006350819331213225852, -0.8709385446395345731, 0.4913509118287982536 ) ) ;
#18119 = VECTOR ( 'NONE', #21975, 1000.000000000000000 ) ;
#18120 = CARTESIAN_POINT ( 'NONE',  ( -7.774884586432871281, 81.99999999999997158, -96.16248895089307780 ) ) ;
#18121 = CARTESIAN_POINT ( 'NONE',  ( 78.73611885933964061, 75.12836414114961769, 3.920034999058580105 ) ) ;
#18122 = CARTESIAN_POINT ( 'NONE',  ( -90.73089019026657809, 70.47975153197518239, 61.57984177518897440 ) ) ;
#18123 = VECTOR ( 'NONE', #6391, 1000.000000000000000 ) ;
#18124 = ORIENTED_EDGE ( 'NONE', *, *, #1441, .T. ) ;
#18125 = CARTESIAN_POINT ( 'NONE',  ( -22.60047370202423167, 329.4438419316639965, 414.4311550204333798 ) ) ;
#18126 = AXIS2_PLACEMENT_3D ( 'NONE', #21175, #19226, #22531 ) ;
#18127 = DIRECTION ( 'NONE',  ( -0.000000000000000000, -1.000000000000000000, 0.000000000000000000 ) ) ;
#18128 = DIRECTION ( 'NONE',  ( 0.01292394549866733230, 0.005513023399720419666, 0.9999012842304692006 ) ) ;
#18129 = EDGE_CURVE ( 'NONE', #12309, #2375, #17361, .T. ) ;
#18130 = ORIENTED_EDGE ( 'NONE', *, *, #3618, .T. ) ;
#18131 = DIRECTION ( 'NONE',  ( 0.01035335185279153900, 0.005513005182355262476, 0.9999312050732647172 ) ) ;
#18132 = DIRECTION ( 'NONE',  ( 0.000000000000000000, 0.000000000000000000, 1.000000000000000000 ) ) ;
#18133 = CARTESIAN_POINT ( 'NONE',  ( 51.99565694909048830, 170.0000000000000284, -0.6720553790413839046 ) ) ;
#18134 = CARTESIAN_POINT ( 'NONE',  ( 92.27487665213190837, 79.82259189700671698, -31.19759217298441811 ) ) ;
#18135 = PLANE ( 'NONE',  #18079 ) ;
#18136 = CARTESIAN_POINT ( 'NONE',  ( -90.99469209931201874, 80.00980328568596178, 31.64094806796596160 ) ) ;
#18137 = DIRECTION ( 'NONE',  ( -7.125109674243555432E-05, 0.9999848031710253382, -0.005512562950850175003 ) ) ;
#18138 = CIRCLE ( 'NONE', #21044, 83.99999999999998579 ) ;
#18139 = ORIENTED_EDGE ( 'NONE', *, *, #6136, .F. ) ;
#18140 = CARTESIAN_POINT ( 'NONE',  ( -11.48960883379135467, 186.2785219672419146, 308.5185337839570252 ) ) ;
#18141 = ADVANCED_FACE ( 'NONE', ( #10350, #14257, #8948 ), #5617, .F. ) ;
#18142 = CARTESIAN_POINT ( 'NONE',  ( -49.97548680510080743, 114.3943234633897390, 167.7607494535559454 ) ) ;
#18143 = CARTESIAN_POINT ( 'NONE',  ( -11.07366896422823288, 186.7668193309826279, 308.3749965093444416 ) ) ;
#18144 = EDGE_LOOP ( 'NONE', ( #19306, #5137, #3957, #3323 ) ) ;
#18145 = CIRCLE ( 'NONE', #21746, 2.499999999999988010 ) ;
#18146 = ORIENTED_EDGE ( 'NONE', *, *, #818, .F. ) ;
#18147 = AXIS2_PLACEMENT_3D ( 'NONE', #5503, #17595, #5382 ) ;
#18148 = CARTESIAN_POINT ( 'NONE',  ( -75.30975508861040169, 94.90914755154933857, 80.17755788556743823 ) ) ;
#18149 = CARTESIAN_POINT ( 'NONE',  ( -12.58378492319879527, 109.7167104967248434, 130.3428598364639299 ) ) ;
#18150 = ITEM_DEFINED_TRANSFORMATION ( 'NONE', 'NONE', #18349,  #6292 ) ;
#18151 = CIRCLE ( 'NONE', #12290, 77.00000000000002842 ) ;
#18152 = CARTESIAN_POINT ( 'NONE',  ( -4.397807287087292849, 165.8073468632632910, 324.7107454954286823 ) ) ;
#18153 = EDGE_CURVE ( 'NONE', #18558, #9131, #20895, .T. ) ;
#18154 = EDGE_CURVE ( 'NONE', #12564, #3568, #18053, .T. ) ;
#18155 = ORIENTED_EDGE ( 'NONE', *, *, #13853, .T. ) ;
#18156 = AXIS2_PLACEMENT_3D ( 'NONE', #2919, #9931, #22200 ) ;
#18157 = CARTESIAN_POINT ( 'NONE',  ( 41.21551227533764461, 121.7015652700166868, 248.5325502308119781 ) ) ;
#18158 = DIRECTION ( 'NONE',  ( 0.4397038457472493556, 0.000000000000000000, -0.8981428216241997831 ) ) ;
#18159 = CARTESIAN_POINT ( 'NONE',  ( -106.3959516824314022, 78.65697569891366925, -27.92701496092233882 ) ) ;
#18160 = CARTESIAN_POINT ( 'NONE',  ( 45.23671757199362986, 168.6025580852140138, 18.02358667753535926 ) ) ;
#18161 = PLANE ( 'NONE',  #10947 ) ;
#18162 = CARTESIAN_POINT ( 'NONE',  ( -11.26897896307171720, 86.89782342943594529, 75.98389258083668096 ) ) ;
#18163 = ORIENTED_EDGE ( 'NONE', *, *, #13445, .T. ) ;
#18164 = CARTESIAN_POINT ( 'NONE',  ( 3.866440703273595680, 70.35631045439365039, -81.75340644824426306 ) ) ;
#18165 = CIRCLE ( 'NONE', #6048, 4.999999999999997335 ) ;
#18166 = DIRECTION ( 'NONE',  ( -0.9999164797902015955, -2.219203356785933794E-15, 0.01292414190464157009 ) ) ;
#18167 = VERTEX_POINT ( 'NONE', #1834 ) ;
#18168 = CIRCLE ( 'NONE', #17074, 2.000000000000001332 ) ;
#18169 = CARTESIAN_POINT ( 'NONE',  ( 41.69668515243814966, 107.1131874321777673, 70.67272545139887541 ) ) ;
#18170 = CARTESIAN_POINT ( 'NONE',  ( -88.17241286529819888, 88.87836946248037862, 52.06316210395358723 ) ) ;
#18171 = SHAPE_DEFINITION_REPRESENTATION ( #21615, #15037 ) ;
#18172 = ORIENTED_EDGE ( 'NONE', *, *, #9281, .F. ) ;
#18173 = CARTESIAN_POINT ( 'NONE',  ( 23.31673526217817027, 141.4150907639734385, 256.4803039161023435 ) ) ;
#18174 = ORIENTED_EDGE ( 'NONE', *, *, #11212, .F. ) ;
#18175 = DIRECTION ( 'NONE',  ( -0.009760756503427874681, 0.9999378516499565217, -0.005387065077610097945 ) ) ;
#18176 = CARTESIAN_POINT ( 'NONE',  ( -35.77069358118216513, 165.3260487394316840, 277.1141618424657054 ) ) ;
#18177 = VECTOR ( 'NONE', #8709, 1000.000000000000000 ) ;
#18178 = CARTESIAN_POINT ( 'NONE',  ( 0.000000000000000000, 0.000000000000000000, 0.000000000000000000 ) ) ;
#18179 = CARTESIAN_POINT ( 'NONE',  ( -41.84548474893134085, 165.9069838518206836, 244.1862188963381755 ) ) ;
#18180 = DIRECTION ( 'NONE',  ( 0.006595249899610063603, 0.8599936914359664897, 0.5102620438256224578 ) ) ;
#18181 = ORIENTED_EDGE ( 'NONE', *, *, #649, .F. ) ;
#18182 = CYLINDRICAL_SURFACE ( 'NONE', #5472, 2.000000000000001332 ) ;
#18183 = ORIENTED_EDGE ( 'NONE', *, *, #22047, .T. ) ;
#18184 = LINE ( 'NONE', #14280, #18721 ) ;
#18185 = CARTESIAN_POINT ( 'NONE',  ( 0.8743530591963392107, 81.99999999999995737, -98.80339646031046641 ) ) ;
#18186 = DIRECTION ( 'NONE',  ( 7.125109674403838460E-05, -0.9999848031710254492, 0.005512562950847868688 ) ) ;
#18187 = DIRECTION ( 'NONE',  ( 0.01292394549866738608, 0.005513023399720468239, 0.9999012842304692006 ) ) ;
#18188 = CARTESIAN_POINT ( 'NONE',  ( -41.56623493000981284, 91.17157287525390075, -82.46967996629571473 ) ) ;
#18189 = DIRECTION ( 'NONE',  ( -0.9999164797902015955, -2.045145117964614424E-15, 0.01292414190464167591 ) ) ;
#18190 = CARTESIAN_POINT ( 'NONE',  ( -54.52327687265812273, 18.00000000000000355, 111.3697098814011923 ) ) ;
#18191 = DIRECTION ( 'NONE',  ( -0.000000000000000000, -1.000000000000000000, -0.000000000000000000 ) ) ;
#18192 = EDGE_LOOP ( 'NONE', ( #13340, #19716, #8116, #20478 ) ) ;
#18193 = EDGE_CURVE ( 'NONE', #7184, #3984, #12192, .T. ) ;
#18194 = CARTESIAN_POINT ( 'NONE',  ( -47.44970423945500926, 167.1338857572628456, 309.0082825445779804 ) ) ;
#18195 = EDGE_LOOP ( 'NONE', ( #7560, #3520, #3299, #8311, #4808 ) ) ;
#18196 = CIRCLE ( 'NONE', #941, 5.000000000000023981 ) ;
#18197 = VERTEX_POINT ( 'NONE', #1620 ) ;
#18198 = ORIENTED_EDGE ( 'NONE', *, *, #6838, .F. ) ;
#18199 = CARTESIAN_POINT ( 'NONE',  ( -85.05069750351505320, 75.00181558815789629, 1.771077756321887797 ) ) ;
#18200 = CARTESIAN_POINT ( 'NONE',  ( -88.16296040167131309, 88.20774758960868667, 52.95573524961071143 ) ) ;
#18202 = VERTEX_POINT ( 'NONE', #343 ) ;
#18201 = ORIENTED_EDGE ( 'NONE', *, *, #7471, .T. ) ;
#18203 = VERTEX_POINT ( 'NONE', #15647 ) ;
#18204 = CARTESIAN_POINT ( 'NONE',  ( 39.50219223099954746, 95.87258117927862600, -43.09091958258431987 ) ) ;
#18205 = CARTESIAN_POINT ( 'NONE',  ( 58.06705108255369652, 143.2435277010459060, 43.50008800685100141 ) ) ;
#18206 = EDGE_CURVE ( 'NONE', #8155, #9852, #5377, .T. ) ;
#18207 = CARTESIAN_POINT ( 'NONE',  ( -72.50839346369934901, 87.61416393227378308, 70.38952438936911449 ) ) ;
#18208 = FACE_OUTER_BOUND ( 'NONE', #15122, .T. ) ;
#18209 = EDGE_CURVE ( 'NONE', #11181, #15659, #10712, .T. ) ;
#18210 = DIRECTION ( 'NONE',  ( -0.1337561903331544455, -0.9909881666746205298, 0.007192708699472569189 ) ) ;
#18211 = AXIS2_PLACEMENT_3D ( 'NONE', #15193, #16696, #20206 ) ;
#18212 = DIRECTION ( 'NONE',  ( -0.01292394549866750231, -0.005513023399722823126, -0.9999012842304692006 ) ) ;
#18213 = CARTESIAN_POINT ( 'NONE',  ( 19.86028698246260404, 182.7578626415639178, 312.8315258640758429 ) ) ;
#18214 = DIRECTION ( 'NONE',  ( 0.01292394549866739996, 0.005513023399721131770, 0.9999012842304692006 ) ) ;
#18215 = CARTESIAN_POINT ( 'NONE',  ( -56.89114125951807210, 144.7594389791736944, 47.47783683149325640 ) ) ;
#18216 = EDGE_CURVE ( 'NONE', #17590, #2480, #22419, .T. ) ;
#18217 = DIRECTION ( 'NONE',  ( 0.9999164797902017066, 2.001050586450180576E-22, -0.01292414190464044946 ) ) ;
#18218 = CARTESIAN_POINT ( 'NONE',  ( -9.995692194476635706, 187.8898849410517471, 308.1575541326492953 ) ) ;
#18219 = EDGE_LOOP ( 'NONE', ( #4720, #411, #9422, #473 ) ) ;
#18220 = VERTEX_POINT ( 'NONE', #12530 ) ;
#18221 = CARTESIAN_POINT ( 'NONE',  ( -29.40402206585521938, 189.4003865961453528, -108.4455932242574505 ) ) ;
#18222 = ADVANCED_FACE ( 'NONE', ( #5268 ), #17711, .F. ) ;
#18223 = DIRECTION ( 'NONE',  ( 0.006717398120142096217, -0.8543148575185137705, 0.5197124212346833083 ) ) ;
#18224 = CARTESIAN_POINT ( 'NONE',  ( 74.88917560116811956, 74.99998524847650572, -1.300231399588960723 ) ) ;
#18225 = CARTESIAN_POINT ( 'NONE',  ( -56.14790736339946164, 143.5743091050289024, 104.9804413797129286 ) ) ;
#18226 = EDGE_CURVE ( 'NONE', #18970, #4876, #16909, .T. ) ;
#18227 = CARTESIAN_POINT ( 'NONE',  ( 78.45092939588570857, 75.19216699751922306, 5.026242266752571020 ) ) ;
#18228 = PLANE ( 'NONE',  #500 ) ;
#18229 = EDGE_CURVE ( 'NONE', #18675, #13755, #11143, .T. ) ;
#18230 = ORIENTED_EDGE ( 'NONE', *, *, #4136, .T. ) ;
#18231 = CARTESIAN_POINT ( 'NONE',  ( -68.71681667565952978, 91.17157287525388654, 85.89527988174785378 ) ) ;
#18232 = CARTESIAN_POINT ( 'NONE',  ( 180.5562823730566322, 0.2186116466668785452, 37.32265611373066605 ) ) ;
#18233 = DIRECTION ( 'NONE',  ( -0.01292394549866738608, -0.005513023399720699824, -0.9999012842304692006 ) ) ;
#18234 = DIRECTION ( 'NONE',  ( 0.01292394549866733230, 0.005513023399720419666, 0.9999012842304692006 ) ) ;
#18235 = DIRECTION ( 'NONE',  ( -0.9999164797902017066, -6.965998958219365988E-18, 0.01292414190464157356 ) ) ;
#18236 = DIRECTION ( 'NONE',  ( 0.9999164797902015955, 2.001050586450180341E-22, -0.01292414190464038874 ) ) ;
#18237 = CARTESIAN_POINT ( 'NONE',  ( 64.99457118636310327, 170.0000000000000284, -0.8400692238017243296 ) ) ;
#18238 = ORIENTED_EDGE ( 'NONE', *, *, #2105, .T. ) ;
#18239 = CARTESIAN_POINT ( 'NONE',  ( 49.46945221206134136, 189.4905266074825647, -93.11355607525817391 ) ) ;
#18240 = DIRECTION ( 'NONE',  ( 0.9999164797902017066, 2.001050586450178931E-22, -0.01292414190464131508 ) ) ;
#18241 = CARTESIAN_POINT ( 'NONE',  ( -15.14040723921782572, 178.5077077566731418, 311.4171169843866664 ) ) ;
#18242 = ORIENTED_EDGE ( 'NONE', *, *, #17265, .T. ) ;
#18243 = ORIENTED_EDGE ( 'NONE', *, *, #3618, .F. ) ;
#18244 = CARTESIAN_POINT ( 'NONE',  ( 48.56920114533915722, 166.9610289984755127, 276.0150354541233924 ) ) ;
#18245 = ADVANCED_FACE ( 'NONE', ( #4230 ), #1548, .T. ) ;
#18246 = CYLINDRICAL_SURFACE ( 'NONE', #10357, 78.99999999999998579 ) ;
#18247 = EDGE_CURVE ( 'NONE', #12598, #12496, #7462, .T. ) ;
#18248 = CIRCLE ( 'NONE', #11280, 126.0000000000000000 ) ;
#18249 = CARTESIAN_POINT ( 'NONE',  ( 9.142505149400571796, 81.19615242270661781, -88.65345271381767134 ) ) ;
#18250 = EDGE_CURVE ( 'NONE', #11360, #14478, #2294, .T. ) ;
#18251 = CARTESIAN_POINT ( 'NONE',  ( 51.50086788761742440, 181.5071008296286266, 255.8949677505804061 ) ) ;
#18252 = ORIENTED_EDGE ( 'NONE', *, *, #14431, .F. ) ;
#18253 = CARTESIAN_POINT ( 'NONE',  ( 82.72602501251986951, 105.0000000000000142, -72.50183911544655757 ) ) ;
#18254 = CARTESIAN_POINT ( 'NONE',  ( -12.64949829888728772, 181.7347035077120267, 322.1854682947845845 ) ) ;
#18255 = ORIENTED_EDGE ( 'NONE', *, *, #11799, .T. ) ;
#18256 = VERTEX_POINT ( 'NONE', #21668 ) ;
#18257 = DIRECTION ( 'NONE',  ( 0.000000000000000000, 1.000000000000000000, -0.000000000000000000 ) ) ;
#18258 = EDGE_LOOP ( 'NONE', ( #8391, #12351, #20738, #5497 ) ) ;
#18259 = FACE_OUTER_BOUND ( 'NONE', #21918, .T. ) ;
#18260 = LINE ( 'NONE', #9520, #20454 ) ;
#18261 = LINE ( 'NONE', #12863, #11451 ) ;
#18262 = ORIENTED_EDGE ( 'NONE', *, *, #7520, .F. ) ;
#18263 = DIRECTION ( 'NONE',  ( -0.01292414190464117457, -5.551059884324760964E-17, -0.9999164797902015955 ) ) ;
#18264 = AXIS2_PLACEMENT_3D ( 'NONE', #1507, #3327, #6664 ) ;
#18265 = CARTESIAN_POINT ( 'NONE',  ( -18.87699466420335170, 140.4778767860208006, 87.01405127310820831 ) ) ;
#18266 = EDGE_CURVE ( 'NONE', #10332, #784, #18261, .T. ) ;
#18267 = EDGE_CURVE ( 'NONE', #21547, #14045, #7678, .T. ) ;
#18268 = ORIENTED_EDGE ( 'NONE', *, *, #1377, .T. ) ;
#18269 = DIRECTION ( 'NONE',  ( -0.4397038457472424167, 0.000000000000000000, -0.8981428216242032248 ) ) ;
#18270 = CARTESIAN_POINT ( 'NONE',  ( -89.37197774827599517, 89.12559863199479082, 51.49225512938619431 ) ) ;
#18271 = PRODUCT_CONTEXT ( 'NONE', #5421, 'mechanical' ) ;
#18272 = VECTOR ( 'NONE', #4370, 1000.000000000000000 ) ;
#18273 = ORIENTED_EDGE ( 'NONE', *, *, #22205, .T. ) ;
#18274 = CARTESIAN_POINT ( 'NONE',  ( 54.52327687265662348, 18.00000000000000355, -111.3697098814019313 ) ) ;
#18275 = CARTESIAN_POINT ( 'NONE',  ( -51.96998430978931083, 113.4377214578606186, -43.52080978029741232 ) ) ;
#18276 = ORIENTED_EDGE ( 'NONE', *, *, #3583, .T. ) ;
#18277 = FACE_OUTER_BOUND ( 'NONE', #21691, .T. ) ;
#18278 = CARTESIAN_POINT ( 'NONE',  ( -162.0000000000000000, 20.00000000000000000, -53.76161406891256433 ) ) ;
#18279 = ORIENTED_EDGE ( 'NONE', *, *, #13327, .T. ) ;
#18280 = DIRECTION ( 'NONE',  ( 0.9999464000778708339, 1.417269118681738664E-05, -0.01035358732233848666 ) ) ;
#18281 = CIRCLE ( 'NONE', #18648, 2.499999999999988010 ) ;
#18282 = CARTESIAN_POINT ( 'NONE',  ( -1.634140231236729024, 188.2752817596284842, 274.5462097314439234 ) ) ;
#18283 = VERTEX_POINT ( 'NONE', #4112 ) ;
#18284 = CARTESIAN_POINT ( 'NONE',  ( -71.36098783483133445, 96.34992515573605942, 81.57916788671384722 ) ) ;
#18285 = VERTEX_POINT ( 'NONE', #16341 ) ;
#18286 = CARTESIAN_POINT ( 'NONE',  ( 48.56361546678319030, 189.3893605493459233, -111.4534788612804732 ) ) ;
#18287 = CARTESIAN_POINT ( 'NONE',  ( 50.79326848830832120, 189.6011149706892525, -73.06981957049683274 ) ) ;
#18288 = CARTESIAN_POINT ( 'NONE',  ( 106.2770331005257134, 84.99999999999997158, -28.37590941890332985 ) ) ;
#18289 = CARTESIAN_POINT ( 'NONE',  ( -0.9951589266573748205, 69.99999999999998579, -76.99356894384553129 ) ) ;
#18290 = DIRECTION ( 'NONE',  ( 0.9999164797902017066, 0.000000000000000000, -0.01292414190464177826 ) ) ;
#18291 = FACE_OUTER_BOUND ( 'NONE', #16314, .T. ) ;
#18292 = VECTOR ( 'NONE', #7753, 1000.000000000000227 ) ;
#18293 = ORIENTED_EDGE ( 'NONE', *, *, #22387, .F. ) ;
#18294 = CARTESIAN_POINT ( 'NONE',  ( 17.14168828271968437, 177.4876913356084174, 88.22687136455920154 ) ) ;
#18295 = ORIENTED_EDGE ( 'NONE', *, *, #9514, .T. ) ;
#18296 = ORIENTED_EDGE ( 'NONE', *, *, #11050, .T. ) ;
#18297 = ORIENTED_EDGE ( 'NONE', *, *, #7942, .F. ) ;
#18298 = CARTESIAN_POINT ( 'NONE',  ( -88.16317630448737930, 88.23127654838400247, 52.93781122257118454 ) ) ;
#18299 = CARTESIAN_POINT ( 'NONE',  ( -10.85567112094788200, 105.6999953372425551, 127.2994028633183348 ) ) ;
#18300 = CARTESIAN_POINT ( 'NONE',  ( -7.586966048391873940, 188.5645970664055255, 275.7666243300806173 ) ) ;
#18301 = AXIS2_PLACEMENT_3D ( 'NONE', #15615, #10988, #12277 ) ;
#18302 = CARTESIAN_POINT ( 'NONE',  ( -18.18280553459775106, 164.2235859539597413, 322.8974543720026418 ) ) ;
#18303 = CARTESIAN_POINT ( 'NONE',  ( 70.11017230969866887, 70.50928942481357353, 84.76194619987022350 ) ) ;
#18304 = ORIENTED_EDGE ( 'NONE', *, *, #3141, .F. ) ;
#18305 = VECTOR ( 'NONE', #1885, 999.9999999999998863 ) ;
#18306 = CARTESIAN_POINT ( 'NONE',  ( -9.995692194476635706, 187.8898849410517471, 308.1575541326492953 ) ) ;
#18307 = PLANE ( 'NONE',  #14472 ) ;
#18308 = CARTESIAN_POINT ( 'NONE',  ( 19.16750076320854035, 183.4954371053536875, 317.5119934807448772 ) ) ;
#18309 = PLANE ( 'NONE',  #12916 ) ;
#18310 = CARTESIAN_POINT ( 'NONE',  ( -59.21412731835795284, 126.5883500096206262, 107.6139730003580581 ) ) ;
#18311 = DIRECTION ( 'NONE',  ( 7.125109674160258889E-05, -0.9999848031710252272, 0.005512562950849897447 ) ) ;
#18312 = VERTEX_POINT ( 'NONE', #2517 ) ;
#18313 = LINE ( 'NONE', #9716, #13889 ) ;
#18314 = VECTOR ( 'NONE', #10764, 999.9999999999998863 ) ;
#18315 = EDGE_CURVE ( 'NONE', #7696, #20154, #6520, .T. ) ;
#18316 = ORIENTED_EDGE ( 'NONE', *, *, #8774, .T. ) ;
#18317 = CARTESIAN_POINT ( 'NONE',  ( 40.92831632140950404, 108.1243619184625828, 71.56358903111998870 ) ) ;
#18318 = EDGE_LOOP ( 'NONE', ( #17473, #13097 ) ) ;
#18319 = CARTESIAN_POINT ( 'NONE',  ( -41.00000899811524846, 169.5540992312279229, 273.1580453575298293 ) ) ;
#18320 = DIRECTION ( 'NONE',  ( 0.000000000000000000, 0.000000000000000000, -1.000000000000000000 ) ) ;
#18321 = FACE_OUTER_BOUND ( 'NONE', #8277, .T. ) ;
#18322 = EDGE_CURVE ( 'NONE', #1264, #22032, #21678, .T. ) ;
#18323 = LINE ( 'NONE', #9608, #9295 ) ;
#18324 = ADVANCED_FACE ( 'NONE', ( #3992, #11017 ), #18046, .F. ) ;
#18325 = ORIENTED_EDGE ( 'NONE', *, *, #169, .T. ) ;
#18326 = FACE_OUTER_BOUND ( 'NONE', #849, .T. ) ;
#18327 = VERTEX_POINT ( 'NONE', #8142 ) ;
#18328 = CARTESIAN_POINT ( 'NONE',  ( 72.63249643174764003, -8.673617379884035472E-16, 144.6929016030553896 ) ) ;
#18329 = CARTESIAN_POINT ( 'NONE',  ( 3.807734317907725430, 166.6242057324384689, 294.5972214811819754 ) ) ;
#18330 = CARTESIAN_POINT ( 'NONE',  ( 45.34042976591830154, 164.1467306581421610, 26.04760348465793385 ) ) ;
#18331 = AXIS2_PLACEMENT_3D ( 'NONE', #19477, #17550, #14463 ) ;
#18332 = CIRCLE ( 'NONE', #6591, 83.99999999999998579 ) ;
#18333 = EDGE_CURVE ( 'NONE', #12374, #14615, #18691, .T. ) ;
#18334 = CYLINDRICAL_SURFACE ( 'NONE', #17253, 2.000000000000001332 ) ;
#18335 = AXIS2_PLACEMENT_3D ( 'NONE', #20076, #2300, #11148 ) ;
#18336 = CARTESIAN_POINT ( 'NONE',  ( 50.34172219119072622, 140.1470953820377474, 26.11528428595510931 ) ) ;
#18337 = ORIENTED_EDGE ( 'NONE', *, *, #15905, .F. ) ;
#18338 = CARTESIAN_POINT ( 'NONE',  ( -55.33837949231439524, 118.9192529882355984, 167.6120857178885899 ) ) ;
#18339 = FACE_OUTER_BOUND ( 'NONE', #13334, .T. ) ;
#18340 = CARTESIAN_POINT ( 'NONE',  ( -14.99641971449742783, 178.7475833985533029, 310.9402587844948584 ) ) ;
#18341 = ORIENTED_EDGE ( 'NONE', *, *, #8979, .T. ) ;
#18342 = EDGE_CURVE ( 'NONE', #16500, #5147, #4664, .T. ) ;
#18343 = CARTESIAN_POINT ( 'NONE',  ( -69.26439091410644266, 97.43560758832659019, 77.57060057039426226 ) ) ;
#18344 = ADVANCED_FACE ( 'NONE', ( #6423 ), #16880, .T. ) ;
#18345 = EDGE_CURVE ( 'NONE', #5948, #12252, #22005, .T. ) ;
#18346 = PRODUCT ( 'Lower Angular Base Cradle Segment', 'Lower Angular Base Cradle Segment', '', ( #18271 ) ) ;
#18347 = VECTOR ( 'NONE', #18725, 1000.000000000000114 ) ;
#18348 = LINE ( 'NONE', #9750, #8493 ) ;
#18349 = AXIS2_PLACEMENT_3D ( 'NONE', #14804, #2482, #12724 ) ;
#18350 = B_SPLINE_CURVE_WITH_KNOTS ( 'NONE', 3,
 ( #21339, #9040, #16094, #16642, #7768, #16515, #5609, #21753, #7221, #13302, #19926, #15022, #11224, #6276 ),
 .UNSPECIFIED., .F., .F.,
 ( 4, 2, 2, 2, 2, 2, 4 ),
 ( 0.000000000000000000, 0.001584441135952660389, 0.003168882271905320777, 0.003961102839881667885, 0.004753323407858014993, 0.005545543975834362101, 0.006337764543810709209 ),
 .UNSPECIFIED. ) ;
#18351 = DIRECTION ( 'NONE',  ( -0.9999164797902015955, -6.965998958219364448E-18, 0.01292414190464157182 ) ) ;
#18352 = EDGE_CURVE ( 'NONE', #17283, #665, #14411, .T. ) ;
#18353 = DIRECTION ( 'NONE',  ( -0.01292394549866738782, -0.005513023399720468239, -0.9999012842304692006 ) ) ;
#18354 = AXIS2_PLACEMENT_3D ( 'NONE', #209, #10885, #556 ) ;
#18355 = FACE_OUTER_BOUND ( 'NONE', #7943, .T. ) ;
#18356 = ORIENTED_EDGE ( 'NONE', *, *, #2649, .F. ) ;
#18357 = ADVANCED_FACE ( 'NONE', ( #13333 ), #13439, .T. ) ;
#18358 = VERTEX_POINT ( 'NONE', #11697 ) ;
#18359 = CARTESIAN_POINT ( 'NONE',  ( 39.39497909003009823, 91.17157287525387233, -85.51628863845822082 ) ) ;
#18360 = ADVANCED_FACE ( 'NONE', ( #18485 ), #2749, .F. ) ;
#18361 = CARTESIAN_POINT ( 'NONE',  ( -15.23197394876478761, 178.3512841404416349, 311.7746290397823259 ) ) ;
#18362 = ORIENTED_EDGE ( 'NONE', *, *, #17039, .F. ) ;
#18363 = FACE_OUTER_BOUND ( 'NONE', #1829, .T. ) ;
#18365 = CARTESIAN_POINT ( 'NONE',  ( -5.156377330703347361, 81.19615242270661781, -99.58697729741749072 ) ) ;
#18364 = CARTESIAN_POINT ( 'NONE',  ( -38.85236994344747075, 97.01168560782741679, 84.15801439602003597 ) ) ;
#18366 = CARTESIAN_POINT ( 'NONE',  ( -41.49766754275730563, 95.16167501252658667, -43.27024962841050382 ) ) ;
#18367 = DIRECTION ( 'NONE',  ( -1.372099599554306628E-14, 0.000000000000000000, 1.000000000000000000 ) ) ;
#18368 = AXIS2_PLACEMENT_3D ( 'NONE', #11421, #630, #11308 ) ;
#18369 = ORIENTED_EDGE ( 'NONE', *, *, #11484, .T. ) ;
#18370 = CARTESIAN_POINT ( 'NONE',  ( -8.201109248996173662, 109.7083723963158519, 128.7736724690130359 ) ) ;
#18371 = AXIS2_PLACEMENT_3D ( 'NONE', #14407, #16245, #16365 ) ;
#18372 =( BOUNDED_SURFACE ( )  B_SPLINE_SURFACE ( 3, 2, ( 
 ( #1514, #15539, #22488 ),
 ( #13401, #20476, #11657 ),
 ( #15345, #17069, #8089 ),
 ( #20371, #1219, #13614 ),
 ( #8213, #22075, #16955 ),
 ( #10047, #1330, #6380 ),
 ( #1093, #22297, #4854 ),
 ( #15244, #6488, #8310 ),
 ( #4734, #11773, #18767 ),
 ( #6588, #3031, #20597 ),
 ( #15123, #4761, #11804 ),
 ( #15269, #22646, #17429 ),
 ( #16989, #10295, #18676 ),
 ( #20394, #15705, #13642 ) ),
 .UNSPECIFIED., .F., .F., .T. ) 
 B_SPLINE_SURFACE_WITH_KNOTS ( ( 4, 2, 2, 2, 2, 2, 4 ),
 ( 3, 3 ),
 ( 6.938893903907228378E-18, 0.001878086432925094810, 0.003756172865850182681, 0.005634259298775270985, 0.007512345731700358423, 0.01126851859755053503, 0.01502469146340070991 ),
 ( 0.000000000000000000, 1.000000000000000000 ),
 .UNSPECIFIED. ) 
 GEOMETRIC_REPRESENTATION_ITEM ( )  RATIONAL_B_SPLINE_SURFACE ( (
 ( 1.000000000000000000, 0.7193398003386572981, 1.000000000000000000),
 ( 1.000000000000000000, 0.7439100388544447329, 1.000000000000000000),
 ( 1.000000000000000000, 0.7665383218960091227, 1.000000000000000000),
 ( 1.000000000000000000, 0.8084046970498726115, 1.000000000000000000),
 ( 1.000000000000000000, 0.8276426232564266794, 1.000000000000000000),
 ( 1.000000000000000000, 0.8630029158315868365, 1.000000000000000000),
 ( 1.000000000000000000, 0.8791524022219731060, 1.000000000000000000),
 ( 1.000000000000000000, 0.9083399791581028282, 1.000000000000000000),
 ( 1.000000000000000000, 0.9212515500168145799, 1.000000000000000000),
 ( 1.000000000000000000, 0.9553996440806984403, 1.000000000000000000),
 ( 1.000000000000000000, 0.9720881558707328285, 1.000000000000000000),
 ( 1.000000000000000000, 0.9943940623865485939, 1.000000000000000000),
 ( 1.000000000000000000, 0.9999834998403251962, 1.000000000000000000),
 ( 1.000000000000000000, 1.000000000000000000, 1.000000000000000000) ) ) 
 REPRESENTATION_ITEM ( '' )  SURFACE ( )  );
#18373 = CARTESIAN_POINT ( 'NONE',  ( 27.99766143412564290, 170.0000000000008242, -0.3618759733291194713 ) ) ;
#18374 = CARTESIAN_POINT ( 'NONE',  ( -4.315545553080795571, 81.44091995301853615, -99.47772690391978756 ) ) ;
#18375 = EDGE_CURVE ( 'NONE', #5742, #18256, #1021, .T. ) ;
#18376 = AXIS2_PLACEMENT_3D ( 'NONE', #15119, #7749, #4284 ) ;
#18377 = VERTEX_POINT ( 'NONE', #2849 ) ;
#18378 = PLANE ( 'NONE',  #2159 ) ;
#18379 = CARTESIAN_POINT ( 'NONE',  ( -88.17087551971840753, 88.81088884623601132, 52.22087021872155077 ) ) ;
#18380 = PRODUCT_CONTEXT ( 'NONE', #10138, 'mechanical' ) ;
#18382 = ORIENTED_EDGE ( 'NONE', *, *, #11458, .F. ) ;
#18381 = VERTEX_POINT ( 'NONE', #11594 ) ;
#18383 = DIRECTION ( 'NONE',  ( -0.000000000000000000, -1.000000000000000000, -0.000000000000000000 ) ) ;
#18384 = VECTOR ( 'NONE', #3058, 999.9999999999998863 ) ;
#18385 = CARTESIAN_POINT ( 'NONE',  ( -52.02336739672247035, 111.7630282158269068, -46.72747482793098328 ) ) ;
#18386 = ORIENTED_EDGE ( 'NONE', *, *, #10434, .T. ) ;
#18387 = CARTESIAN_POINT ( 'NONE',  ( 4.195452682864946325, 166.7895964344300808, 324.5942600080963985 ) ) ;
#18388 = AXIS2_PLACEMENT_3D ( 'NONE', #8278, #8376, #17234 ) ;
#18389 = DIRECTION ( 'NONE',  ( -0.1296504907605108559, -0.005475273188901296634, -0.9915446392518419971 ) ) ;
#18390 = CIRCLE ( 'NONE', #8460, 2.999999999999988898 ) ;
#18391 = FACE_OUTER_BOUND ( 'NONE', #8710, .T. ) ;
#18392 = DIRECTION ( 'NONE',  ( -0.000000000000000000, -1.000000000000000000, -0.000000000000000000 ) ) ;
#18393 = CARTESIAN_POINT ( 'NONE',  ( -55.33980451424918101, 138.9189490516561136, 167.5018344588715138 ) ) ;
#18394 = EDGE_LOOP ( 'NONE', ( #19476, #19702, #18009, #4611 ) ) ;
#18395 = EDGE_CURVE ( 'NONE', #1815, #5416, #18588, .T. ) ;
#18396 = CARTESIAN_POINT ( 'NONE',  ( -1.163172771417702700, 37.00000000000000711, -89.99248318111824574 ) ) ;
#18397 = AXIS2_PLACEMENT_3D ( 'NONE', #2039, #433, #7550 ) ;
#18398 = ORIENTED_EDGE ( 'NONE', *, *, #10753, .T. ) ;
#18399 = LINE ( 'NONE', #5987, #9589 ) ;
#18400 = CARTESIAN_POINT ( 'NONE',  ( 50.92554597170246211, 189.6011917897851617, -73.05759422026605421 ) ) ;
#18401 = CARTESIAN_POINT ( 'NONE',  ( -14.56978029430814026, 147.5825162344054888, 276.9379655111616785 ) ) ;
#18402 = CARTESIAN_POINT ( 'NONE',  ( -22.53299579847311307, 324.7083362324482323, 307.5570220811381432 ) ) ;
#18403 = VERTEX_POINT ( 'NONE', #21745 ) ;
#18404 = CARTESIAN_POINT ( 'NONE',  ( -44.67419437013135308, 164.7531598149646470, 277.2324002234482236 ) ) ;
#18405 = CARTESIAN_POINT ( 'NONE',  ( -50.72033869335580647, 114.2302237440943742, 169.5554601261313223 ) ) ;
#18406 = ADVANCED_BREP_SHAPE_REPRESENTATION ( '', ( #17564, #6292 ), #20590 ) ;
#18407 = ORIENTED_EDGE ( 'NONE', *, *, #4136, .F. ) ;
#18408 = CIRCLE ( 'NONE', #20587, 95.00000000000001421 ) ;
#18409 = CARTESIAN_POINT ( 'NONE',  ( -1.163172771417702700, 30.00000000000000711, -89.99248318111824574 ) ) ;
#18410 = EDGE_CURVE ( 'NONE', #10488, #1018, #17322, .T. ) ;
#18411 = EDGE_LOOP ( 'NONE', ( #8518, #4002, #13330, #16068 ) ) ;
#18412 = VECTOR ( 'NONE', #17349, 999.9999999999998863 ) ;
#18413 = CARTESIAN_POINT ( 'NONE',  ( 3.316624388958365088, 166.4147108432491109, 256.6009726804241495 ) ) ;
#18414 = CARTESIAN_POINT ( 'NONE',  ( -90.17346960859786975, 87.02965620341086606, 51.38002018875397425 ) ) ;
#18415 = VECTOR ( 'NONE', #17207, 1000.000000000000000 ) ;
#18416 = ORIENTED_EDGE ( 'NONE', *, *, #8572, .T. ) ;
#18417 = CARTESIAN_POINT ( 'NONE',  ( 51.07319921393753503, 94.45452722260040446, 82.70828171889813518 ) ) ;
#18418 = LINE ( 'NONE', #3167, #1061 ) ;
#18419 = CARTESIAN_POINT ( 'NONE',  ( -63.96182961141723666, 99.65143692054147095, 75.28401729384056296 ) ) ;
#18420 = DIRECTION ( 'NONE',  ( -0.9999164797902015955, -4.476705744456278510E-15, 0.01292414190464144692 ) ) ;
#18421 = VECTOR ( 'NONE', #6187, 1000.000000000000000 ) ;
#18422 = CARTESIAN_POINT ( 'NONE',  ( -89.33746586332897266, 79.97654757638649414, -29.19326486971738532 ) ) ;
#18423 = VECTOR ( 'NONE', #13342, 999.9999999999998863 ) ;
#18424 = DIRECTION ( 'NONE',  ( 0.009760756503428011724, -0.9999378516499566327, 0.005387065077610982654 ) ) ;
#18425 = CARTESIAN_POINT ( 'NONE',  ( -12.58378492319879527, 109.7167104967248434, 130.3428598364639299 ) ) ;
#18426 = EDGE_CURVE ( 'NONE', #17671, #8789, #12926, .T. ) ;
#18427 = ORIENTED_EDGE ( 'NONE', *, *, #20735, .T. ) ;
#18428 = EDGE_CURVE ( 'NONE', #22554, #850, #20239, .T. ) ;
#18429 = LINE ( 'NONE', #2695, #6952 ) ;
#18430 = DIRECTION ( 'NONE',  ( -0.01292394549866740169, -0.005513023399719847208, -0.9999012842304693116 ) ) ;
#18431 = CARTESIAN_POINT ( 'NONE',  ( 20.16092468778748170, 182.5150849490638620, 317.5062687794200542 ) ) ;
#18432 = CARTESIAN_POINT ( 'NONE',  ( -40.58111162538312300, 119.0295134562300063, 187.4227113448806961 ) ) ;
#18433 = DIRECTION ( 'NONE',  ( -0.9999164797902015955, -6.965998958219364448E-18, 0.01292414190464157182 ) ) ;
#18434 = CONICAL_SURFACE ( 'NONE', #21342, 2.499999999999988010, 1.029744258676651425 ) ;
#18435 = DIRECTION ( 'NONE',  ( -0.01292414190464044772, 0.000000000000000000, -0.9999164797902015955 ) ) ;
#18436 = CARTESIAN_POINT ( 'NONE',  ( 64.42259306105445660, 139.7551263635816952, -45.17031240767400391 ) ) ;
#18437 = ORIENTED_EDGE ( 'NONE', *, *, #12969, .T. ) ;
#18439 = CARTESIAN_POINT ( 'NONE',  ( 4.376210989365964643, 81.97459999999998104, -92.29796090835097289 ) ) ;
#18438 = CIRCLE ( 'NONE', #15147, 126.0000000000000000 ) ;
#18440 = ORIENTED_EDGE ( 'NONE', *, *, #13721, .F. ) ;
#18441 = ORIENTED_EDGE ( 'NONE', *, *, #21003, .F. ) ;
#18442 = AXIS2_PLACEMENT_3D ( 'NONE', #17461, #12169, #19154 ) ;
#18443 = PRODUCT_DEFINITION ( 'UNKNOWN', '', #14343, #14104 ) ;
#18444 = CARTESIAN_POINT ( 'NONE',  ( -6.702556532201372264, 69.99999999999998579, -87.68700545388549017 ) ) ;
#18445 = EDGE_LOOP ( 'NONE', ( #15321, #20847, #21846, #1681 ) ) ;
#18446 = VERTEX_POINT ( 'NONE', #11101 ) ;
#18447 = AXIS2_PLACEMENT_3D ( 'NONE', #10559, #1946, #15867 ) ;
#18448 = CARTESIAN_POINT ( 'NONE',  ( 77.67389597125436751, 75.11017898543126137, -5.579058506725625755 ) ) ;
#18449 = FACE_OUTER_BOUND ( 'NONE', #2915, .T. ) ;
#18450 = CARTESIAN_POINT ( 'NONE',  ( 10.98841023064628075, 180.4221386788646839, 76.40681165563029253 ) ) ;
#18451 = ADVANCED_FACE ( 'NONE', ( #9472 ), #22058, .F. ) ;
#18452 = CARTESIAN_POINT ( 'NONE',  ( 45.23618318876806654, 176.1024441089967070, 17.98224245540398769 ) ) ;
#18453 = VERTEX_POINT ( 'NONE', #7537 ) ;
#18454 = LINE ( 'NONE', #21860, #11347 ) ;
#18455 = ORIENTED_EDGE ( 'NONE', *, *, #9466, .T. ) ;
#18456 = DIRECTION ( 'NONE',  ( 1.000000000000000000, 0.000000000000000000, 0.000000000000000000 ) ) ;
#18457 = CARTESIAN_POINT ( 'NONE',  ( -64.14629883989944403, 91.30780077822167584, 66.46930053661340310 ) ) ;
#18458 = AXIS2_PLACEMENT_3D ( 'NONE', #20399, #8131, #6064 ) ;
#18459 = PLANE ( 'NONE',  #3839 ) ;
#18460 = VECTOR ( 'NONE', #4647, 999.9999999999998863 ) ;
#18461 = CARTESIAN_POINT ( 'NONE',  ( 91.08520856931308174, 77.44390114805533187, -31.69197020849773239 ) ) ;
#18462 = DIRECTION ( 'NONE',  ( -0.000000000000000000, -1.000000000000000000, 0.000000000000000000 ) ) ;
#18463 = CARTESIAN_POINT ( 'NONE',  ( 49.00729593383175597, 189.4940257501801568, -92.47283438282913437 ) ) ;
#18464 = VERTEX_POINT ( 'NONE', #20140 ) ;
#18465 = CARTESIAN_POINT ( 'NONE',  ( -56.11438623100832501, 126.5883500096206262, 107.5739081604536693 ) ) ;
#18466 = CARTESIAN_POINT ( 'NONE',  ( -13.42770478899201514, 180.9551723136957264, 307.9573190744438875 ) ) ;
#18467 = VERTEX_POINT ( 'NONE', #18225 ) ;
#18468 = ORIENTED_EDGE ( 'NONE', *, *, #7379, .F. ) ;
#18469 = EDGE_CURVE ( 'NONE', #16395, #11456, #9603, .T. ) ;
#18470 = AXIS2_PLACEMENT_3D ( 'NONE', #648, #16745, #15017 ) ;
#18471 = AXIS2_PLACEMENT_3D ( 'NONE', #6735, #13761, #16996 ) ;
#18472 = CARTESIAN_POINT ( 'NONE',  ( -68.24431907518334128, 70.78648125535667646, 86.27145290589803039 ) ) ;
#18473 = VERTEX_POINT ( 'NONE', #21855 ) ;
#18474 = DIRECTION ( 'NONE',  ( 7.125109674161238737E-05, -0.9999848031710253382, 0.005512562950850163727 ) ) ;
#18475 = AXIS2_PLACEMENT_3D ( 'NONE', #12404, #14137, #12177 ) ;
#18476 = AXIS2_PLACEMENT_3D ( 'NONE', #4868, #11908, #3154 ) ;
#18477 = EDGE_CURVE ( 'NONE', #444, #7056, #10727, .T. ) ;
#18478 = EDGE_LOOP ( 'NONE', ( #3353, #12713, #15324, #5412, #9192, #2320, #10227, #13898 ) ) ;
#18479 = CARTESIAN_POINT ( 'NONE',  ( 12.78096684794300941, 190.5101800092401731, 307.8461504866875202 ) ) ;
#18480 = ADVANCED_FACE ( 'NONE', ( #18449 ), #16402, .T. ) ;
#18481 = CARTESIAN_POINT ( 'NONE',  ( -8.523216527044569446, 185.4125284852929099, 305.1540476800932424 ) ) ;
#18482 = ORIENTED_EDGE ( 'NONE', *, *, #19705, .T. ) ;
#18483 = CARTESIAN_POINT ( 'NONE',  ( -106.8724933792760652, 79.04398536104956463, -26.04362031086678897 ) ) ;
#18484 = CARTESIAN_POINT ( 'NONE',  ( -106.1636641531658398, 79.04398536104955042, 28.79715981783285628 ) ) ;
#18485 = FACE_OUTER_BOUND ( 'NONE', #16809, .T. ) ;
#18486 = AXIS2_PLACEMENT_3D ( 'NONE', #8298, #8069, #6797 ) ;
#18487 = ORIENTED_EDGE ( 'NONE', *, *, #20310, .T. ) ;
#18488 = AXIS2_PLACEMENT_3D ( 'NONE', #19921, #4296, #9368 ) ;
#18489 = DIRECTION ( 'NONE',  ( 0.9726991065672924153, 0.2316562896908775926, -0.01384960395994898341 ) ) ;
#18490 = CARTESIAN_POINT ( 'NONE',  ( 0.000000000000000000, 23.00000000000000000, -120.0000000000000000 ) ) ;
#18491 = ADVANCED_FACE ( 'NONE', ( #6150 ), #4294, .T. ) ;
#18492 = ADVANCED_FACE ( 'NONE', ( #16635 ), #15513, .T. ) ;
#18493 = ORIENTED_EDGE ( 'NONE', *, *, #20741, .T. ) ;
#18494 = AXIS2_PLACEMENT_3D ( 'NONE', #15312, #22368, #11621 ) ;
#18495 = DIRECTION ( 'NONE',  ( -0.9999164797902015955, -2.001050586450178695E-22, 0.01292414190464131335 ) ) ;
#18496 = DIRECTION ( 'NONE',  ( -7.125109674160258889E-05, 0.9999848031710252272, -0.005512562950849896580 ) ) ;
#18497 = EDGE_CURVE ( 'NONE', #10627, #16835, #12822, .T. ) ;
#18498 = PRODUCT_CONTEXT ( 'NONE', #16035, 'mechanical' ) ;
#18499 = AXIS2_PLACEMENT_3D ( 'NONE', #2871, #13236, #15722 ) ;
#18500 = ORIENTED_EDGE ( 'NONE', *, *, #15700, .F. ) ;
#18501 = VECTOR ( 'NONE', #22054, 1000.000000000000227 ) ;
#18502 = LINE ( 'NONE', #823, #3628 ) ;
#18503 = CARTESIAN_POINT ( 'NONE',  ( -50.76749586831994066, 109.7796205288052107, -46.01748440586237621 ) ) ;
#18504 = CARTESIAN_POINT ( 'NONE',  ( 10.85296234298433404, 174.5781088801995793, 324.4652677311569278 ) ) ;
#18505 = DIRECTION ( 'NONE',  ( 0.000000000000000000, 1.000000000000000000, -0.000000000000000000 ) ) ;
#18506 = LINE ( 'NONE', #2767, #18088 ) ;
#18507 = CARTESIAN_POINT ( 'NONE',  ( -51.99565694909051672, 170.0000000000000284, 0.6720553790413400508 ) ) ;
#18508 = CARTESIAN_POINT ( 'NONE',  ( -44.26142469380095434, 168.8134312302532862, 57.43298357076854899 ) ) ;
#18509 = FACE_OUTER_BOUND ( 'NONE', #21167, .T. ) ;
#18510 = EDGE_LOOP ( 'NONE', ( #1529, #146, #4676 ) ) ;
#18511 = ADVANCED_FACE ( 'NONE', ( #9727 ), #5885, .T. ) ;
#18512 = CARTESIAN_POINT ( 'NONE',  ( 65.91440269377942229, 105.0000000000000000, 70.32555938675403695 ) ) ;
#18513 = VERTEX_POINT ( 'NONE', #2818 ) ;
#18514 = CARTESIAN_POINT ( 'NONE',  ( -14.53239793090661180, 175.6255473142593644, 113.6490011371711688 ) ) ;
#18515 =( BOUNDED_SURFACE ( )  B_SPLINE_SURFACE ( 3, 2, ( 
 ( #1172, #11273, #2664 ),
 ( #18718, #8165, #6096 ),
 ( #16794, #4688, #1046 ),
 ( #833, #22257, #13023 ) ),
 .UNSPECIFIED., .F., .F., .T. ) 
 B_SPLINE_SURFACE_WITH_KNOTS ( ( 4, 4 ),
 ( 3, 3 ),
 ( 5.799006443144740786, 5.860583945225279479 ),
 ( 0.000000000000000000, 1.000000000000000000 ),
 .UNSPECIFIED. ) 
 GEOMETRIC_REPRESENTATION_ITEM ( )  RATIONAL_B_SPLINE_SURFACE ( (
 ( 1.000000000000000000, 0.9016180287879261845, 1.000000000000000000),
 ( 1.000000000000000000, 0.9034913259101577943, 1.000000000000000000),
 ( 1.000000000000000000, 0.9052491015987668144, 1.000000000000000000),
 ( 1.000000000000000000, 0.9068900557993655465, 1.000000000000000000) ) ) 
 REPRESENTATION_ITEM ( '' )  SURFACE ( )  );
#18516 = CARTESIAN_POINT ( 'NONE',  ( 153.9999999999992610, 18.00000000000000355, 53.76161406891468175 ) ) ;
#18517 = VECTOR ( 'NONE', #8015, 999.9999999999998863 ) ;
#18518 = CYLINDRICAL_SURFACE ( 'NONE', #8687, 10.99999999999999289 ) ;
#18519 = CARTESIAN_POINT ( 'NONE',  ( -9.809641362382286900, 69.99999999999998579, -87.34492244913440118 ) ) ;
#18520 = CARTESIAN_POINT ( 'NONE',  ( 83.82126922308901840, 105.0000000000000000, -71.23197895489381892 ) ) ;
#18521 = CARTESIAN_POINT ( 'NONE',  ( 0.000000000000000000, 0.000000000000000000, 0.000000000000000000 ) ) ;
#18522 = EDGE_LOOP ( 'NONE', ( #15191, #15383, #14911, #18468, #12517 ) ) ;
#18523 = CONICAL_SURFACE ( 'NONE', #10446, 14.99999999999997691, 0.03490658503988662564 ) ;
#18524 = CARTESIAN_POINT ( 'NONE',  ( -48.80449223365644684, 105.5072037373731888, 92.81729778463858338 ) ) ;
#18525 = FACE_OUTER_BOUND ( 'NONE', #4604, .T. ) ;
#18526 = VERTEX_POINT ( 'NONE', #8539 ) ;
#18527 = DIRECTION ( 'NONE',  ( -7.125109674403850657E-05, 0.9999848031710253382, -0.005512562950847868688 ) ) ;
#18528 =( REPRESENTATION_RELATIONSHIP ('NONE','NONE', #11808, #10182 ) REPRESENTATION_RELATIONSHIP_WITH_TRANSFORMATION ( #8690 )SHAPE_REPRESENTATION_RELATIONSHIP( ) );
#18529 = CARTESIAN_POINT ( 'NONE',  ( -88.16267813286435739, 88.17648390085673782, 52.97871766249971159 ) ) ;
#18530 = ADVANCED_FACE ( 'NONE', ( #8221, #4742 ), #8097, .T. ) ;
#18531 = ORIENTED_EDGE ( 'NONE', *, *, #18352, .T. ) ;
#18532 = B_SPLINE_CURVE_WITH_KNOTS ( 'NONE', 3,
 ( #3380, #15687, #5733, #4126, #22629, #1770, #19223, #12765, #17522, #702 ),
 .UNSPECIFIED., .F., .F.,
 ( 4, 2, 2, 2, 4 ),
 ( 0.000000000000000000, 0.0004486304370347037745, 0.0008972608740694075491, 0.001345891311104094410, 0.001794521748138781271 ),
 .UNSPECIFIED. ) ;
#18533 = CARTESIAN_POINT ( 'NONE',  ( -67.77252605414460618, 99.53959963624815543, 78.34284531778030214 ) ) ;
#18534 = FACE_OUTER_BOUND ( 'NONE', #10235, .T. ) ;
#18535 = DIRECTION ( 'NONE',  ( -0.9999164797902015955, -6.965998958219364448E-18, 0.01292414190464157182 ) ) ;
#18536 = CARTESIAN_POINT ( 'NONE',  ( -88.18246585727159470, 88.96524493581522108, 50.92653801520322787 ) ) ;
#18537 = LINE ( 'NONE', #8196, #502 ) ;
#18538 = EDGE_CURVE ( 'NONE', #12722, #15597, #10371, .T. ) ;
#18539 = LINE ( 'NONE', #9913, #519 ) ;
#18540 = EDGE_CURVE ( 'NONE', #5654, #10387, #9257, .T. ) ;
#18541 = ORIENTED_EDGE ( 'NONE', *, *, #20378, .F. ) ;
#18542 = ORIENTED_EDGE ( 'NONE', *, *, #4719, .T. ) ;
#18543 = LINE ( 'NONE', #20700, #11000 ) ;
#18544 = CARTESIAN_POINT ( 'NONE',  ( 13.77150744767909352, 159.1779288738256923, 324.5124548241344655 ) ) ;
#18545 = CARTESIAN_POINT ( 'NONE',  ( 20.49956196390964891, 182.0660229792639768, 312.5168992756803732 ) ) ;
#18546 = CARTESIAN_POINT ( 'NONE',  ( 93.07689643981107963, 77.12912189501255966, 28.79946631983735728 ) ) ;
#18547 = CARTESIAN_POINT ( 'NONE',  ( 66.07231611197045140, 94.48610424851698042, 82.54302267323384967 ) ) ;
#18548 = ORIENTED_EDGE ( 'NONE', *, *, #3608, .T. ) ;
#18549 = PRODUCT ( 'Jaw', 'Jaw', '', ( #8359 ) ) ;
#18550 = DIRECTION ( 'NONE',  ( -0.1337561903331558333, -0.9909881666746205298, 0.007192708699472581332 ) ) ;
#18551 = CARTESIAN_POINT ( 'NONE',  ( 0.000000000000000000, 45.00000000000000711, -96.00000000000000000 ) ) ;
#18552 = VERTEX_POINT ( 'NONE', #11558 ) ;
#18553 = CARTESIAN_POINT ( 'NONE',  ( -5.055008945778654450, 172.7557180373005679, 323.6808309321652928 ) ) ;
#18554 = EDGE_LOOP ( 'NONE', ( #9272, #5909, #18094, #4601 ) ) ;
#18555 = CARTESIAN_POINT ( 'NONE',  ( 48.31072223536580879, 166.8507685304811048, 256.0170097695140043 ) ) ;
#18556 = EDGE_CURVE ( 'NONE', #22275, #6959, #2923, .T. ) ;
#18557 = EDGE_CURVE ( 'NONE', #17537, #19075, #8112, .T. ) ;
#18558 = VERTEX_POINT ( 'NONE', #4972 ) ;
#18559 = CARTESIAN_POINT ( 'NONE',  ( -86.79222083800951282, 104.3814432989690602, -67.58039954014913064 ) ) ;
#18560 = CIRCLE ( 'NONE', #212, 87.00000000000001421 ) ;
#18561 = CARTESIAN_POINT ( 'NONE',  ( 105.4610200154982067, 77.75225708752515175, -31.27258767819551721 ) ) ;
#18562 = LINE ( 'NONE', #18452, #5241 ) ;
#18563 = CARTESIAN_POINT ( 'NONE',  ( 12.87400438914988321, 189.0062672177662364, 276.1925613188200828 ) ) ;
#18564 =( LENGTH_UNIT ( ) NAMED_UNIT ( * ) SI_UNIT ( .MILLI., .METRE. ) );
#18565 = CARTESIAN_POINT ( 'NONE',  ( -47.41909850602771570, 108.0982075334647163, 200.0025971627301260 ) ) ;
#18566 = PLANE ( 'NONE',  #3060 ) ;
#18567 = LINE ( 'NONE', #6277, #13754 ) ;
#18568 = FACE_OUTER_BOUND ( 'NONE', #3091, .T. ) ;
#18569 = FACE_OUTER_BOUND ( 'NONE', #20675, .T. ) ;
#18570 = CARTESIAN_POINT ( 'NONE',  ( 50.52662230413528732, 189.4876967392748384, -93.64056134612683024 ) ) ;
#18571 = ORIENTED_EDGE ( 'NONE', *, *, #7074, .F. ) ;
#18572 = DIRECTION ( 'NONE',  ( -0.1296504907605104673, -0.005475273188900901117, -0.9915446392518421082 ) ) ;
#18573 = CARTESIAN_POINT ( 'NONE',  ( -13.02319649578260119, 181.4398012765341832, 307.4785573789200157 ) ) ;
#18574 = ORIENTED_EDGE ( 'NONE', *, *, #4292, .T. ) ;
#18575 = ORIENTED_EDGE ( 'NONE', *, *, #15837, .T. ) ;
#18576 = ORIENTED_EDGE ( 'NONE', *, *, #19142, .T. ) ;
#18577 = ADVANCED_FACE ( 'NONE', ( #6387 ), #15354, .F. ) ;
#18578 = CARTESIAN_POINT ( 'NONE',  ( 13.64212105858742241, 187.1241579171488070, 322.8665338120699744 ) ) ;
#18579 = VERTEX_POINT ( 'NONE', #12002 ) ;
#18580 = CARTESIAN_POINT ( 'NONE',  ( 0.1403038029401039999, 327.3197362253691836, 312.1404394970679164 ) ) ;
#18581 = CARTESIAN_POINT ( 'NONE',  ( 6.781388072971601844, 37.00000000000000711, -83.91926714759891581 ) ) ;
#18582 = DIRECTION ( 'NONE',  ( 1.386679829960243376E-14, -0.000000000000000000, 1.000000000000000000 ) ) ;
#18583 = ORIENTED_EDGE ( 'NONE', *, *, #12205, .F. ) ;
#18584 = CARTESIAN_POINT ( 'NONE',  ( 12.62937233005813908, 190.5670816176184132, 307.8363845662464087 ) ) ;
#18585 = CARTESIAN_POINT ( 'NONE',  ( -15.51253772856980362, 177.8410551567861830, 313.5641263009300701 ) ) ;
#18586 = CARTESIAN_POINT ( 'NONE',  ( -106.2089377515398780, 77.28919246392742082, -28.62973177816245496 ) ) ;
#18587 = DIRECTION ( 'NONE',  ( 0.9999164797902015955, 2.001050586450181282E-22, -0.01292414190463992731 ) ) ;
#18588 = LINE ( 'NONE', #14799, #4817 ) ;
#18589 = EDGE_LOOP ( 'NONE', ( #22401, #11342, #21514, #4036 ) ) ;
#18590 = CARTESIAN_POINT ( 'NONE',  ( -6.702556532201369599, 95.03750572909316929, -87.68700545388549017 ) ) ;
#18591 = ORIENTED_EDGE ( 'NONE', *, *, #4000, .T. ) ;
#18592 = CARTESIAN_POINT ( 'NONE',  ( -52.60896573992756942, 111.9218655255082382, -46.77848885693064318 ) ) ;
#18593 = EDGE_CURVE ( 'NONE', #2627, #17705, #18884, .T. ) ;
#18594 = CARTESIAN_POINT ( 'NONE',  ( -9.483901319675773323, 187.1048918696979229, 307.9736811914152668 ) ) ;
#18595 = ORIENTED_EDGE ( 'NONE', *, *, #7562, .F. ) ;
#18596 = EDGE_CURVE ( 'NONE', #11284, #10697, #22305, .T. ) ;
#18597 = LINE ( 'NONE', #20317, #1079 ) ;
#18598 = CARTESIAN_POINT ( 'NONE',  ( -10.85980368455889433, 163.6991139211620236, 126.9796742121690443 ) ) ;
#18599 = EDGE_LOOP ( 'NONE', ( #1187, #13225, #16099, #8597 ) ) ;
#18600 = CARTESIAN_POINT ( 'NONE',  ( 90.46801631146688294, 78.10499069285118878, -32.69910015975909090 ) ) ;
#18601 = EDGE_LOOP ( 'NONE', ( #14110, #3313, #21443, #9763 ) ) ;
#18602 = CARTESIAN_POINT ( 'NONE',  ( 1.117803423002110774, 45.00000000000000000, 109.6947150755565161 ) ) ;
#18603 = DIRECTION ( 'NONE',  ( -0.9999164797902017066, -2.001050586450178931E-22, 0.01292414190464131508 ) ) ;
#18604 = DIRECTION ( 'NONE',  ( -5.440186201345738641E-18, -1.000000000000000000, -1.334940939666364181E-17 ) ) ;
#18605 = DIRECTION ( 'NONE',  ( -0.9999164797902015955, 0.000000000000000000, 0.01292414190464162733 ) ) ;
#18606 = DIRECTION ( 'NONE',  ( -0.9999164797902015955, -6.965998958219364448E-18, 0.01292414190464157182 ) ) ;
#18607 = EDGE_CURVE ( 'NONE', #8361, #559, #7047, .T. ) ;
#18608 = ORIENTED_EDGE ( 'NONE', *, *, #11747, .F. ) ;
#18609 = DIRECTION ( 'NONE',  ( 0.01292414190464179213, 0.000000000000000000, 0.9999164797902017066 ) ) ;
#18610 = VERTEX_POINT ( 'NONE', #1229 ) ;
#18611 = CARTESIAN_POINT ( 'NONE',  ( 1.054933926688728762, 165.4499317482979279, 81.61824794009152129 ) ) ;
#18612 = DIRECTION ( 'NONE',  ( 7.125109674160325297E-05, -0.9999848031710253382, 0.005512562950849327591 ) ) ;
#18613 = CARTESIAN_POINT ( 'NONE',  ( 54.52327687265664480, 0.000000000000000000, 111.3697098814019029 ) ) ;
#18614 = DIRECTION ( 'NONE',  ( 0.01292394549866738608, 0.005513023399720699824, 0.9999012842304692006 ) ) ;
#18615 = AXIS2_PLACEMENT_3D ( 'NONE', #13719, #18974, #3231 ) ;
#18616 = EDGE_CURVE ( 'NONE', #2170, #4358, #19151, .T. ) ;
#18617 = EDGE_LOOP ( 'NONE', ( #16140, #16698, #10671, #13083 ) ) ;
#18618 = FACE_OUTER_BOUND ( 'NONE', #8802, .T. ) ;
#18619 = DIRECTION ( 'NONE',  ( 0.01292394549866738782, 0.005513023399720468239, 0.9999012842304692006 ) ) ;
#18620 = EDGE_LOOP ( 'NONE', ( #3129, #17254, #184, #20957, #3267 ) ) ;
#18621 = CARTESIAN_POINT ( 'NONE',  ( 49.05359984820991315, 95.50335886808198893, -45.57402858099457177 ) ) ;
#18622 = DIRECTION ( 'NONE',  ( 0.9999164797902015955, 6.965998958219364448E-18, -0.01292414190464157182 ) ) ;
#18623 = ORIENTED_EDGE ( 'NONE', *, *, #3526, .F. ) ;
#18624 = EDGE_CURVE ( 'NONE', #18579, #7423, #18438, .T. ) ;
#18625 = CARTESIAN_POINT ( 'NONE',  ( -55.33808647217894361, 114.8068154851947753, 167.6347561330238420 ) ) ;
#18626 = CARTESIAN_POINT ( 'NONE',  ( -88.16489327553765065, 88.40164337095862379, 52.78994026756070923 ) ) ;
#18627 = EDGE_CURVE ( 'NONE', #20328, #5755, #6758, .T. ) ;
#18628 = EDGE_CURVE ( 'NONE', #14863, #4193, #18532, .T. ) ;
#18629 = CARTESIAN_POINT ( 'NONE',  ( -70.91392079944854743, 91.17157287525390075, -84.09052168258642723 ) ) ;
#18630 = EDGE_CURVE ( 'NONE', #14680, #1627, #19739, .T. ) ;
#18631 = ORIENTED_EDGE ( 'NONE', *, *, #12390, .F. ) ;
#18632 = AXIS2_PLACEMENT_3D ( 'NONE', #3105, #6455, #1397 ) ;
#18633 = CARTESIAN_POINT ( 'NONE',  ( 41.19638261157624015, 121.2962013336460956, 247.0525242307099347 ) ) ;
#18634 = DIRECTION ( 'NONE',  ( 7.125109674160258889E-05, -0.9999848031710252272, 0.005512562950849896580 ) ) ;
#18635 = CARTESIAN_POINT ( 'NONE',  ( -52.54962939365285735, 114.3681980354872962, 163.0548411849881063 ) ) ;
#18636 = CARTESIAN_POINT ( 'NONE',  ( -55.33894950108811628, 126.9191314136040063, 167.5679852142817197 ) ) ;
#18637 = DIRECTION ( 'NONE',  ( 0.01292414190464130988, 0.000000000000000000, 0.9999164797902017066 ) ) ;
#18638 = CARTESIAN_POINT ( 'NONE',  ( -52.18379134969580235, 189.4892127681350189, -92.03799725394125630 ) ) ;
#18639 = EDGE_LOOP ( 'NONE', ( #17506, #6483, #17939, #19831, #14500, #8640, #18548, #18052, #17456, #7816 ) ) ;
#18640 = DIRECTION ( 'NONE',  ( -0.01292414190464131335, -1.358703943142685684E-38, -0.9999164797902015955 ) ) ;
#18641 = PLANE ( 'NONE',  #7087 ) ;
#18642 = CARTESIAN_POINT ( 'NONE',  ( 88.95538863342427760, 79.66477516473727860, -30.55627054544669363 ) ) ;
#18643 = CARTESIAN_POINT ( 'NONE',  ( -59.76742335808221895, 114.2164937952198187, 165.2669475732469380 ) ) ;
#18644 = CARTESIAN_POINT ( 'NONE',  ( -10.98162931145840027, 147.1570210637436560, 278.5494351491892076 ) ) ;
#18645 = EDGE_CURVE ( 'NONE', #12921, #17177, #7785, .T. ) ;
#18646 = ORIENTED_EDGE ( 'NONE', *, *, #9642, .T. ) ;
#18647 = CYLINDRICAL_SURFACE ( 'NONE', #3333, 87.00000000000001421 ) ;
#18648 = AXIS2_PLACEMENT_3D ( 'NONE', #6949, #15710, #8902 ) ;
#18649 = DIRECTION ( 'NONE',  ( -0.01292394549866741904, -0.005513023399721091004, -0.9999012842304693116 ) ) ;
#18650 = CARTESIAN_POINT ( 'NONE',  ( -64.02091254583170610, 100.1262683277930989, 76.17020158700519517 ) ) ;
#18651 = ORIENTED_EDGE ( 'NONE', *, *, #21990, .F. ) ;
#18652 = EDGE_LOOP ( 'NONE', ( #2756, #5727, #10540, #22199, #3665 ) ) ;
#18653 = EDGE_LOOP ( 'NONE', ( #15924, #15220, #16323, #1153 ) ) ;
#18654 = CARTESIAN_POINT ( 'NONE',  ( 163.9999999999992610, 20.00000000000000000, -53.76161406891485228 ) ) ;
#18655 = EDGE_CURVE ( 'NONE', #17624, #10072, #5197, .T. ) ;
#18656 = AXIS2_PLACEMENT_3D ( 'NONE', #4689, #6451, #13463 ) ;
#18657 = EDGE_LOOP ( 'NONE', ( #19562, #10192, #14144, #7608, #8638, #16334, #17128, #19652, #3803, #3330, #22258, #595 ) ) ;
#18658 = CARTESIAN_POINT ( 'NONE',  ( -90.06143632372041452, 71.82810837149287408, 60.05335399799299978 ) ) ;
#18659 = VECTOR ( 'NONE', #4607, 1000.000000000000000 ) ;
#18660 = CARTESIAN_POINT ( 'NONE',  ( 105.7099399341924766, 78.83711888896351638, -30.42080736548479436 ) ) ;
#18661 = DIRECTION ( 'NONE',  ( 1.000000000000000000, -0.000000000000000000, 1.362186893977296347E-14 ) ) ;
#18662 = CARTESIAN_POINT ( 'NONE',  ( 15.56728057410850852, 187.6694373681214927, 276.3106296452654078 ) ) ;
#18663 = ORIENTED_EDGE ( 'NONE', *, *, #15237, .F. ) ;
#18664 = CARTESIAN_POINT ( 'NONE',  ( 41.08943404267284905, 95.79007946549236863, 84.02896320188966683 ) ) ;
#18665 = FACE_OUTER_BOUND ( 'NONE', #16707, .T. ) ;
#18666 = CARTESIAN_POINT ( 'NONE',  ( -39.06500206180663071, 108.1243619184625118, 72.59752038349127190 ) ) ;
#18667 = CARTESIAN_POINT ( 'NONE',  ( -90.00000000000000000, 45.00100000000000477, 8.394090934816448357E-16 ) ) ;
#18668 = EDGE_CURVE ( 'NONE', #1318, #8537, #14036, .T. ) ;
#18669 = CARTESIAN_POINT ( 'NONE',  ( 93.58499681124563097, 69.99999999999998579, 57.80872228166916926 ) ) ;
#18670 = AXIS2_PLACEMENT_3D ( 'NONE', #10745, #19236, #7403 ) ;
#18671 = ORIENTED_EDGE ( 'NONE', *, *, #20711, .T. ) ;
#18672 = CARTESIAN_POINT ( 'NONE',  ( 14.14167086503323034, 113.6998737626107641, 126.9321988120954643 ) ) ;
#18673 = CARTESIAN_POINT ( 'NONE',  ( -8.248824808275418974, 185.5853417291986887, 308.0251062239191810 ) ) ;
#18674 = AXIS2_PLACEMENT_3D ( 'NONE', #17015, #2858, #14952 ) ;
#18675 = VERTEX_POINT ( 'NONE', #18173 ) ;
#18676 = CARTESIAN_POINT ( 'NONE',  ( -3.143027085112847896, 189.9554771204651900, 275.0835221995262714 ) ) ;
#18677 = ORIENTED_EDGE ( 'NONE', *, *, #20455, .F. ) ;
#18678 = B_SPLINE_CURVE_WITH_KNOTS ( 'NONE', 3,
 ( #15508, #4569, #11598, #13443, #6749, #2854, #22129, #22236, #6430, #18925, #9865, #16885 ),
 .UNSPECIFIED., .F., .F.,
 ( 4, 2, 2, 2, 2, 4 ),
 ( 0.000000000000000000, 0.003508523874122990941, 0.007017047748245981882, 0.01052557162236897673, 0.01227983355943047111, 0.01403409549649196376 ),
 .UNSPECIFIED. ) ;
#18679 = CARTESIAN_POINT ( 'NONE',  ( 15.75623612227090575, 186.0822479155119140, 322.5113043239726380 ) ) ;
#18680 = CIRCLE ( 'NONE', #6937, 2.000000000000000000 ) ;
#18681 = LINE ( 'NONE', #19013, #873 ) ;
#18682 = MECHANICAL_DESIGN_GEOMETRIC_PRESENTATION_REPRESENTATION (  '', ( #8763 ), #5473 ) ;
#18683 = CARTESIAN_POINT ( 'NONE',  ( 9.196690372329099361, 142.8086146031528187, 274.7267082784171066 ) ) ;
#18684 = AXIS2_PLACEMENT_3D ( 'NONE', #15439, #5239, #17453 ) ;
#18685 = CARTESIAN_POINT ( 'NONE',  ( 65.44029839719591735, 190.1904397277867531, 33.64500428368677376 ) ) ;
#18686 = CARTESIAN_POINT ( 'NONE',  ( -14.80339701313337386, 179.0542959306228568, 310.3963275995649838 ) ) ;
#18687 = ADVANCED_FACE ( 'NONE', ( #18062 ), #17412, .T. ) ;
#18688 = PLANE ( 'NONE',  #7413 ) ;
#18689 = ADVANCED_FACE ( 'NONE', ( #14080 ), #19105, .F. ) ;
#18690 = CARTESIAN_POINT ( 'NONE',  ( -20.57109388430227881, 136.7551719540686008, -44.05520973278501629 ) ) ;
#18691 = LINE ( 'NONE', #15285, #17696 ) ;
#18692 = VERTEX_POINT ( 'NONE', #2308 ) ;
#18693 = CARTESIAN_POINT ( 'NONE',  ( 83.58290648752347352, 104.4142135623730638, 71.51152175067952044 ) ) ;
#18694 = DIRECTION ( 'NONE',  ( -5.440186201345738641E-18, -1.000000000000000000, -1.334940939666364181E-17 ) ) ;
#18695 = DIRECTION ( 'NONE',  ( -0.01292394549866750231, -0.005513023399722823126, -0.9999012842304692006 ) ) ;
#18696 = CARTESIAN_POINT ( 'NONE',  ( -52.60896573992756942, 111.9218655255082382, -46.77848885693064318 ) ) ;
#18697 = CIRCLE ( 'NONE', #1465, 85.00000000000002842 ) ;
#18698 = CIRCLE ( 'NONE', #20166, 85.00000000000001421 ) ;
#18699 = CARTESIAN_POINT ( 'NONE',  ( -28.40747727069632589, 324.0565921083061198, 312.5274174544723564 ) ) ;
#18700 = CARTESIAN_POINT ( 'NONE',  ( -16.77435518417359717, 141.3748088146942621, 249.6913015425559195 ) ) ;
#18701 = PRODUCT_DEFINITION ( 'UNKNOWN', '', #13242, #10186 ) ;
#18702 = DIRECTION ( 'NONE',  ( 0.000000000000000000, 0.000000000000000000, 1.000000000000000000 ) ) ;
#18703 = VECTOR ( 'NONE', #12983, 999.9999999999998863 ) ;
#18704 = SHAPE_DEFINITION_REPRESENTATION ( #19488, #10922 ) ;
#18705 = VERTEX_POINT ( 'NONE', #171 ) ;
#18706 = FACE_OUTER_BOUND ( 'NONE', #21, .T. ) ;
#18707 = CARTESIAN_POINT ( 'NONE',  ( -51.12349514068515077, 113.1361128394719771, -43.53008790071018552 ) ) ;
#18708 = CARTESIAN_POINT ( 'NONE',  ( 23.22251776072470619, 138.3748544051812246, 249.1908735552227938 ) ) ;
#18709 = CARTESIAN_POINT ( 'NONE',  ( -51.99565694909051672, 170.0000000000000284, 0.6720553790413400508 ) ) ;
#18710 = CARTESIAN_POINT ( 'NONE',  ( -54.52327687265815115, 20.00000000000000000, -111.3697098814011781 ) ) ;
#18711 = B_SPLINE_CURVE_WITH_KNOTS ( 'NONE', 3,
 ( #4140, #9078, #16586, #2546, #18185, #21808 ),
 .UNSPECIFIED., .F., .F.,
 ( 4, 2, 4 ),
 ( 2.380730968155625444E-07, 0.002629065763328323601, 0.005257893453559830781 ),
 .UNSPECIFIED. ) ;
#18712 = CARTESIAN_POINT ( 'NONE',  ( -44.75523122589896019, 161.1026720614313774, 19.22810367108447238 ) ) ;
#18713 = PRODUCT_DEFINITION_SHAPE ( 'NONE', 'NONE',  #22685 ) ;
#18714 = DIRECTION ( 'NONE',  ( 0.01035335185279138807, 0.005513005182356417802, 0.9999312050732649393 ) ) ;
#18715 = AXIS2_PLACEMENT_3D ( 'NONE', #3402, #1691, #19246 ) ;
#18716 = ADVANCED_FACE ( 'NONE', ( #3598 ), #594, .T. ) ;
#18717 = ORIENTED_EDGE ( 'NONE', *, *, #10497, .T. ) ;
#18718 = CARTESIAN_POINT ( 'NONE',  ( 36.93353118842156135, 92.00280690338281886, -84.44237658585842610 ) ) ;
#18719 = ORIENTED_EDGE ( 'NONE', *, *, #12375, .T. ) ;
#18720 = DIRECTION ( 'NONE',  ( 0.01292414190464174703, 0.000000000000000000, 0.9999164797902015955 ) ) ;
#18721 = VECTOR ( 'NONE', #3687, 1000.000000000000114 ) ;
#18722 = LINE ( 'NONE', #13360, #10053 ) ;
#18723 = AXIS2_PLACEMENT_3D ( 'NONE', #2721, #653, #14921 ) ;
#18724 = CARTESIAN_POINT ( 'NONE',  ( -40.86170866251428180, 168.8134312302532862, 57.38904148829276863 ) ) ;
#18725 = DIRECTION ( 'NONE',  ( 0.1136178953597579422, -0.9935164314186355483, 0.004009283626633659663 ) ) ;
#18726 = ADVANCED_FACE ( 'NONE', ( #21572 ), #18077, .T. ) ;
#18727 = FACE_OUTER_BOUND ( 'NONE', #10280, .T. ) ;
#18728 = DIRECTION ( 'NONE',  ( -0.01292414190464039048, -1.902755938799529063E-22, -0.9999164797902017066 ) ) ;
#18729 = AXIS2_PLACEMENT_3D ( 'NONE', #753, #11087, #5904 ) ;
#18730 = ORIENTED_EDGE ( 'NONE', *, *, #14262, .F. ) ;
#18731 = CARTESIAN_POINT ( 'NONE',  ( 49.36348188940251447, 95.91501852516964277, -46.25422087729876353 ) ) ;
#18732 = CARTESIAN_POINT ( 'NONE',  ( 19.43877198876942813, 177.6144908738019694, 111.1987526180507047 ) ) ;
#18733 = ORIENTED_EDGE ( 'NONE', *, *, #6888, .T. ) ;
#18734 = AXIS2_PLACEMENT_3D ( 'NONE', #21157, #19551, #262 ) ;
#18735 = DIRECTION ( 'NONE',  ( 0.9999164797902017066, 2.219212769279110820E-15, -0.01292414190464157182 ) ) ;
#18736 = AXIS2_PLACEMENT_3D ( 'NONE', #14095, #2234, #186 ) ;
#18737 = EDGE_CURVE ( 'NONE', #724, #8008, #17340, .T. ) ;
#18738 = CARTESIAN_POINT ( 'NONE',  ( -90.09747616180477792, 88.49262567217745357, 52.75167656980727315 ) ) ;
#18739 = VERTEX_POINT ( 'NONE', #8880 ) ;
#18740 = ADVANCED_FACE ( 'NONE', ( #20823 ), #15926, .T. ) ;
#18741 = CARTESIAN_POINT ( 'NONE',  ( -8.991637549221998427, 184.9283712355567104, 323.2327844428430126 ) ) ;
#18742 = AXIS2_PLACEMENT_3D ( 'NONE', #3528, #5698, #7309 ) ;
#18743 = DIRECTION ( 'NONE',  ( 7.125109674161246868E-05, -0.9999848031710252272, 0.005512562950850154186 ) ) ;
#18744 = CARTESIAN_POINT ( 'NONE',  ( -8.680576889647097616, 86.44926012997954956, -75.23049865080909626 ) ) ;
#18745 = DIRECTION ( 'NONE',  ( 2.025474946048326158E-22, -1.000000000000000000, 1.876735158486679638E-22 ) ) ;
#18746 = CARTESIAN_POINT ( 'NONE',  ( -88.16651712116340889, 88.54264735233917349, 52.64450902266127486 ) ) ;
#18747 = DIRECTION ( 'NONE',  ( 1.362186893977296031E-14, 0.000000000000000000, -1.000000000000000000 ) ) ;
#18748 = DIRECTION ( 'NONE',  ( -0.01292394549866632963, -0.005513023399716958026, -0.9999012842304692006 ) ) ;
#18749 = ORIENTED_EDGE ( 'NONE', *, *, #11201, .T. ) ;
#18750 = EDGE_LOOP ( 'NONE', ( #12478, #20779, #2497, #8149 ) ) ;
#18751 = DIRECTION ( 'NONE',  ( -2.459148776294495979E-24, 1.000000000000000000, -1.902597020224326827E-22 ) ) ;
#18752 = CARTESIAN_POINT ( 'NONE',  ( -10.82440428556347101, 109.7167354332198812, 130.3246429589757156 ) ) ;
#18753 = CARTESIAN_POINT ( 'NONE',  ( 91.15750879531701401, 79.10636023297638530, -28.80946033575594356 ) ) ;
#18754 = PLANE ( 'NONE',  #9212 ) ;
#18755 = EDGE_CURVE ( 'NONE', #20552, #20838, #11833, .T. ) ;
#18756 = AXIS2_PLACEMENT_3D ( 'NONE', #11860, #18622, #1406 ) ;
#18757 = EDGE_CURVE ( 'NONE', #14478, #18024, #17737, .T. ) ;
#18758 = DIRECTION ( 'NONE',  ( 0.9999164797902017066, 2.001050586450178931E-22, -0.01292414190464131508 ) ) ;
#18759 =( NAMED_UNIT ( * ) PLANE_ANGLE_UNIT ( ) SI_UNIT ( $, .RADIAN. ) );
#18760 = SURFACE_STYLE_USAGE ( .BOTH. , #7773 ) ;
#18761 = AXIS2_PLACEMENT_3D ( 'NONE', #17856, #9076, #17958 ) ;
#18762 = VECTOR ( 'NONE', #5869, 999.9999999999998863 ) ;
#18763 = B_SPLINE_CURVE_WITH_KNOTS ( 'NONE', 3,
 ( #15337, #8406, #4724, #20467, #5064, #10379, #18642, #15671, #11760, #10151, #11648, #17156, #1427, #18753, #15450, #4957, #9918, #6696 ),
 .UNSPECIFIED., .F., .F.,
 ( 4, 2, 2, 2, 2, 2, 2, 2, 4 ),
 ( 0.000000000000000000, 0.0007972436847030646423, 0.001594487369406129285, 0.002391731054109193927, 0.003188974738812258569, 0.003986218423515323211, 0.004783462108218387854, 0.005580705792921452496, 0.006377949477624517138 ),
 .UNSPECIFIED. ) ;
#18764 = CIRCLE ( 'NONE', #20954, 8.000000000000000000 ) ;
#18765 = DIRECTION ( 'NONE',  ( 7.125109674161246868E-05, -0.9999848031710252272, 0.005512562950850154186 ) ) ;
#18766 = ORIENTED_EDGE ( 'NONE', *, *, #12537, .T. ) ;
#18767 = CARTESIAN_POINT ( 'NONE',  ( -8.569456489635145502, 187.5482121046341319, 277.4292011265865767 ) ) ;
#18768 = ORIENTED_EDGE ( 'NONE', *, *, #15808, .F. ) ;
#18769 = ORIENTED_EDGE ( 'NONE', *, *, #7942, .T. ) ;
#18770 = EDGE_CURVE ( 'NONE', #959, #9955, #9875, .T. ) ;
#18771 = DIRECTION ( 'NONE',  ( -0.01292394549866704608, -0.005513023399720698957, -0.9999012842304692006 ) ) ;
#18772 = CIRCLE ( 'NONE', #6668, 110.0000000000000000 ) ;
#18773 = EDGE_LOOP ( 'NONE', ( #6524, #12302 ) ) ;
#18774 = VECTOR ( 'NONE', #21316, 1000.000000000000114 ) ;
#18775 = ADVANCED_FACE ( 'NONE', ( #20084 ), #1215, .T. ) ;
#18776 = CARTESIAN_POINT ( 'NONE',  ( -1.163172771417702700, 81.99999999999998579, -89.99248318111824574 ) ) ;
#18777 = AXIS2_PLACEMENT_3D ( 'NONE', #18709, #9877, #22579 ) ;
#18778 = CARTESIAN_POINT ( 'NONE',  ( 81.48578126947279543, 75.19548211375456503, 5.038671026100010053 ) ) ;
#18779 = CARTESIAN_POINT ( 'NONE',  ( -41.41899454747532161, 166.0889136240114681, 277.1829612759436827 ) ) ;
#18780 = AXIS2_PLACEMENT_3D ( 'NONE', #11867, #10481, #10370 ) ;
#18781 = DIRECTION ( 'NONE',  ( -5.440186201345738641E-18, -1.000000000000000000, -1.334940939666364181E-17 ) ) ;
#18782 = ORIENTED_EDGE ( 'NONE', *, *, #1910, .T. ) ;
#18783 = CARTESIAN_POINT ( 'NONE',  ( -38.77137772201017185, 125.3750519639578727, 250.0638336716716310 ) ) ;
#18784 = DIRECTION ( 'NONE',  ( 0.000000000000000000, 1.000000000000000000, -0.000000000000000000 ) ) ;
#18785 = DIRECTION ( 'NONE',  ( 0.01292394549866738782, 0.005513023399720700692, 0.9999012842304693116 ) ) ;
#18786 = FACE_OUTER_BOUND ( 'NONE', #15197, .T. ) ;
#18787 = EDGE_CURVE ( 'NONE', #956, #2170, #12214, .T. ) ;
#18788 = EDGE_CURVE ( 'NONE', #18866, #15083, #11090, .T. ) ;
#18789 = CARTESIAN_POINT ( 'NONE',  ( -48.91807906390275207, 94.48610424851698042, 84.02929899226762700 ) ) ;
#18791 = DIRECTION ( 'NONE',  ( 0.01292394549866738608, 0.005513023399720699824, 0.9999012842304692006 ) ) ;
#18790 = DIRECTION ( 'NONE',  ( 5.440186201345738641E-18, 1.000000000000000000, 1.334940939666364181E-17 ) ) ;
#18792 = ORIENTED_EDGE ( 'NONE', *, *, #3754, .F. ) ;
#18793 = AXIS2_PLACEMENT_3D ( 'NONE', #13950, #17633, #11156 ) ;
#18794 = AXIS2_PLACEMENT_3D ( 'NONE', #14458, #2376, #2248 ) ;
#18795 = EDGE_LOOP ( 'NONE', ( #5001, #20707, #8135 ) ) ;
#18796 = FACE_OUTER_BOUND ( 'NONE', #9800, .T. ) ;
#18797 = CARTESIAN_POINT ( 'NONE',  ( -8.380575353881514644, 185.4992511567469080, 308.0384472719858309 ) ) ;
#18798 = ORIENTED_EDGE ( 'NONE', *, *, #11782, .T. ) ;
#18799 = CARTESIAN_POINT ( 'NONE',  ( 7.055447609860087788, 70.09252763182291801, -85.92399523110741200 ) ) ;
#18800 = ORIENTED_EDGE ( 'NONE', *, *, #21724, .F. ) ;
#18801 = AXIS2_PLACEMENT_3D ( 'NONE', #12060, #6871, #17023 ) ;
#18802 = CARTESIAN_POINT ( 'NONE',  ( -55.37125936483477773, 126.9053488551047053, 165.0682320037055320 ) ) ;
#18803 = ADVANCED_FACE ( 'NONE', ( #3434 ), #10336, .T. ) ;
#18804 = VECTOR ( 'NONE', #10666, 1000.000000000000000 ) ;
#18805 = CIRCLE ( 'NONE', #17732, 101.0000000000000000 ) ;
#18806 = DIRECTION ( 'NONE',  ( 7.125109674161246868E-05, -0.9999848031710252272, 0.005512562950850154186 ) ) ;
#18807 = CARTESIAN_POINT ( 'NONE',  ( 13.68126522347680485, 144.1100395844905222, 275.5440367720843824 ) ) ;
#18808 = DIRECTION ( 'NONE',  ( 7.125109674161246868E-05, -0.9999848031710253382, 0.005512562950850155054 ) ) ;
#18809 = ADVANCED_FACE ( 'NONE', ( #17347 ), #13891, .T. ) ;
#18810 = CARTESIAN_POINT ( 'NONE',  ( 68.31397436809166379, 127.4153035195791119, 255.9758934117053570 ) ) ;
#18811 = ORIENTED_EDGE ( 'NONE', *, *, #13175, .F. ) ;
#18812 = AXIS2_PLACEMENT_3D ( 'NONE', #21660, #18582, #16543 ) ;
#18813 = DIRECTION ( 'NONE',  ( 0.01292394549866731149, 0.005513023399720593139, 0.9999012842304692006 ) ) ;
#18814 = CARTESIAN_POINT ( 'NONE',  ( 42.57010254367627766, 108.0286580773774148, 198.5854920750244901 ) ) ;
#18815 = ORIENTED_EDGE ( 'NONE', *, *, #19238, .F. ) ;
#18816 = DIRECTION ( 'NONE',  ( 0.01292414190464038701, 0.000000000000000000, 0.9999164797902017066 ) ) ;
#18817 = CARTESIAN_POINT ( 'NONE',  ( -39.42082737383935154, 91.17157287525388654, 83.51645567887779009 ) ) ;
#18818 = CYLINDRICAL_SURFACE ( 'NONE', #6619, 2.000000000000001332 ) ;
#18819 = TOROIDAL_SURFACE ( 'NONE', #14457, 4.400000000000000355, 0.4000000000000000222 ) ;
#18820 = AXIS2_PLACEMENT_3D ( 'NONE', #9129, #12607, #5450 ) ;
#18821 = DIRECTION ( 'NONE',  ( 0.000000000000000000, 0.000000000000000000, -1.000000000000000000 ) ) ;
#18822 = CARTESIAN_POINT ( 'NONE',  ( 42.57338467509045188, 108.0982075334647163, 198.8394243913123489 ) ) ;
#18823 = DIRECTION ( 'NONE',  ( -0.9999164797902015955, -4.653667080246435885E-16, 0.01292414190464177999 ) ) ;
#18824 = EDGE_CURVE ( 'NONE', #8679, #11415, #10216, .T. ) ;
#18825 = SHAPE_DEFINITION_REPRESENTATION ( #751, #14914 ) ;
#18826 = ADVANCED_FACE ( 'NONE', ( #1492 ), #1605, .F. ) ;
#18827 = CIRCLE ( 'NONE', #14825, 93.00000000000001421 ) ;
#18828 = AXIS2_PLACEMENT_3D ( 'NONE', #15694, #10857, #7277 ) ;
#18830 = ORIENTED_EDGE ( 'NONE', *, *, #18616, .F. ) ;
#18829 = EDGE_LOOP ( 'NONE', ( #2815, #12659, #6349, #17855 ) ) ;
#18831 = CARTESIAN_POINT ( 'NONE',  ( -50.63964423113515778, 108.5889086405974240, -43.51127046276314303 ) ) ;
#18832 = CARTESIAN_POINT ( 'NONE',  ( 13.11455560745687876, 190.2624259001582345, 320.8439992888508527 ) ) ;
#18833 = FACE_OUTER_BOUND ( 'NONE', #19999, .T. ) ;
#18834 = DIRECTION ( 'NONE',  ( 0.7944560844389304544, 0.000000000000000000, 0.6073216033519334145 ) ) ;
#18835 = AXIS2_PLACEMENT_3D ( 'NONE', #12217, #14172, #5394 ) ;
#18836 = DIRECTION ( 'NONE',  ( -2.025474946048326158E-22, 1.000000000000000000, -1.876735158486679638E-22 ) ) ;
#18837 = FACE_OUTER_BOUND ( 'NONE', #11805, .T. ) ;
#18838 = VERTEX_POINT ( 'NONE', #22577 ) ;
#18839 = CARTESIAN_POINT ( 'NONE',  ( 51.57037466492827349, 109.8957517466449048, -44.83956295643738343 ) ) ;
#18840 = ORIENTED_EDGE ( 'NONE', *, *, #17599, .T. ) ;
#18841 = CARTESIAN_POINT ( 'NONE',  ( -9.472248412593195610, 81.99999999999998579, -86.53426659026914081 ) ) ;
#18842 = CARTESIAN_POINT ( 'NONE',  ( 106.0703656581358558, 70.66226986180332403, 29.13909619158252085 ) ) ;
#18843 = DIRECTION ( 'NONE',  ( 0.9999164797902015955, 6.965998958219364448E-18, -0.01292414190464157182 ) ) ;
#18844 = CARTESIAN_POINT ( 'NONE',  ( -39.42082737383935154, 69.99999999999998579, 83.51645567887779009 ) ) ;
#18845 = PLANE ( 'NONE',  #5289 ) ;
#18846 = AXIS2_PLACEMENT_3D ( 'NONE', #4255, #21482, #487 ) ;
#18847 = ORIENTED_EDGE ( 'NONE', *, *, #22107, .F. ) ;
#18848 = DIRECTION ( 'NONE',  ( -0.01292394549866738608, -0.005513023399720699824, -0.9999012842304692006 ) ) ;
#18849 = DIRECTION ( 'NONE',  ( -0.9999164797902017066, -2.001050586450179636E-22, 0.01292414190464131508 ) ) ;
#18850 = ORIENTED_EDGE ( 'NONE', *, *, #5824, .F. ) ;
#18851 = VECTOR ( 'NONE', #18606, 1000.000000000000000 ) ;
#18852 = AXIS2_PLACEMENT_3D ( 'NONE', #8615, #1632, #8717 ) ;
#18853 = CARTESIAN_POINT ( 'NONE',  ( -37.04493930154655601, 165.7286083383001198, 308.8815467460659647 ) ) ;
#18854 = CARTESIAN_POINT ( 'NONE',  ( -88.16512445317465563, 88.42243553698295955, 52.76943054571153624 ) ) ;
#18855 = ORIENTED_EDGE ( 'NONE', *, *, #18477, .T. ) ;
#18856 = ORIENTED_EDGE ( 'NONE', *, *, #8835, .F. ) ;
#18857 = CARTESIAN_POINT ( 'NONE',  ( -73.00030478232707765, 95.66452290628956234, 82.28581592040848136 ) ) ;
#18858 = FACE_OUTER_BOUND ( 'NONE', #271, .T. ) ;
#18859 = DIRECTION ( 'NONE',  ( 0.9999164797902017066, 2.001050586450177285E-22, -0.01292414190464218071 ) ) ;
#18860 = AXIS2_PLACEMENT_3D ( 'NONE', #5266, #17709, #14148 ) ;
#18861 = CARTESIAN_POINT ( 'NONE',  ( -88.16543417756993506, 88.45405585956656580, 52.74322918111940339 ) ) ;
#18862 = CARTESIAN_POINT ( 'NONE',  ( -89.99335928417744412, 79.29537036754121004, 29.40900737050176517 ) ) ;
#18863 = CARTESIAN_POINT ( 'NONE',  ( -52.54463837782685687, 189.4882857640628799, -92.20149275433632852 ) ) ;
#18864 = EDGE_LOOP ( 'NONE', ( #7288, #1741 ) ) ;
#18865 = ORIENTED_EDGE ( 'NONE', *, *, #18070, .T. ) ;
#18866 = VERTEX_POINT ( 'NONE', #12298 ) ;
#18867 = CARTESIAN_POINT ( 'NONE',  ( -64.64902924016615771, 145.1470193978925636, 27.57399779023469932 ) ) ;
#18868 = VECTOR ( 'NONE', #15588, 1000.000000000000000 ) ;
#18869 = CARTESIAN_POINT ( 'NONE',  ( -59.02935498760711397, 114.5067879355092089, 163.4878558818826662 ) ) ;
#18870 = AXIS2_PLACEMENT_3D ( 'NONE', #16737, #759, #13166 ) ;
#18871 = CARTESIAN_POINT ( 'NONE',  ( -13.16231198119108114, 149.0364497547966494, 278.8421488773936403 ) ) ;
#18872 = DIRECTION ( 'NONE',  ( 1.000000000000000000, 0.000000000000000000, 0.000000000000000000 ) ) ;
#18873 = FACE_OUTER_BOUND ( 'NONE', #6731, .T. ) ;
#18874 = CARTESIAN_POINT ( 'NONE',  ( -38.46706438352712354, 69.99999999999998579, 85.27439087629282710 ) ) ;
#18875 = ORIENTED_EDGE ( 'NONE', *, *, #11055, .T. ) ;
#18876 = STYLED_ITEM ( 'NONE', ( #19434 ), #9541 ) ;
#18877 = VERTEX_POINT ( 'NONE', #8471 ) ;
#18878 = CARTESIAN_POINT ( 'NONE',  ( -90.04217887881287652, 70.01937035445752144, 63.21555236838661784 ) ) ;
#18879 = EDGE_CURVE ( 'NONE', #13637, #5948, #5024, .T. ) ;
#18881 = ORIENTED_EDGE ( 'NONE', *, *, #93, .F. ) ;
#18880 = EDGE_LOOP ( 'NONE', ( #14919, #14334, #2124, #20068 ) ) ;
#18882 = EDGE_CURVE ( 'NONE', #165, #4699, #3190, .T. ) ;
#18883 = CARTESIAN_POINT ( 'NONE',  ( -1.390668784055079922E-14, 45.00000000000000000, -110.1134477342067299 ) ) ;
#18884 = LINE ( 'NONE', #13407, #4483 ) ;
#18885 = CARTESIAN_POINT ( 'NONE',  ( -108.7507233931858082, 76.71731347669778245, -17.16766896971221712 ) ) ;
#18886 = DIRECTION ( 'NONE',  ( 0.01292394549866740343, 0.005513023399721065851, 0.9999012842304692006 ) ) ;
#18887 = CARTESIAN_POINT ( 'NONE',  ( 19.70989040611666709, 186.5267750472335422, 276.1911881219696738 ) ) ;
#18888 = ORIENTED_EDGE ( 'NONE', *, *, #22239, .F. ) ;
#18889 = AXIS2_PLACEMENT_3D ( 'NONE', #6667, #19063, #5042 ) ;
#18890 = DIRECTION ( 'NONE',  ( 0.9999164797902017066, 6.965998958219365988E-18, -0.01292414190464157356 ) ) ;
#18891 = CARTESIAN_POINT ( 'NONE',  ( -51.60252166286891651, 189.5983001498699423, -72.25694281118451556 ) ) ;
#18892 = ADVANCED_FACE ( 'NONE', ( #15409 ), #9634, .F. ) ;
#18893 = CARTESIAN_POINT ( 'NONE',  ( 90.51848467603717552, 80.22648697776341464, -32.24949179442774039 ) ) ;
#18894 = EDGE_CURVE ( 'NONE', #726, #13165, #20881, .T. ) ;
#18895 = CARTESIAN_POINT ( 'NONE',  ( 45.23671757199362986, 168.6025580852140138, 18.02358667753535926 ) ) ;
#18896 = ORIENTED_EDGE ( 'NONE', *, *, #12164, .T. ) ;
#18897 = ADVANCED_FACE ( 'NONE', ( #8830 ), #12572, .T. ) ;
#18898 = VERTEX_POINT ( 'NONE', #1386 ) ;
#18899 = CARTESIAN_POINT ( 'NONE',  ( 93.21002351426729149, 72.00000000000000000, 28.79774562292276840 ) ) ;
#18900 = DIRECTION ( 'NONE',  ( 7.125109674160325297E-05, -0.9999848031710252272, 0.005512562950849327591 ) ) ;
#18901 = ORIENTED_EDGE ( 'NONE', *, *, #4449, .T. ) ;
#18902 = B_SPLINE_CURVE_WITH_KNOTS ( 'NONE', 3,
 ( #3173, #8571, #10196, #22557, #1473, #8452, #15502, #6963, #6743, #13767, #19022, #3284, #6849, #13870, #5115, #12150, #17443, #8674 ),
 .UNSPECIFIED., .F., .F.,
 ( 4, 2, 2, 2, 2, 2, 2, 2, 4 ),
 ( 3.469446951953613804E-18, 0.01374954366077128440, 0.02062431549115692139, 0.02406170140634973989, 0.02749908732154255492, 0.04124863098231382197, 0.04812340281269945202, 0.05156078872789227746, 0.05499817464308508902 ),
 .UNSPECIFIED. ) ;
#18903 = CARTESIAN_POINT ( 'NONE',  ( 9.142505149400571796, 70.80384757729338219, -88.65345271381767134 ) ) ;
#18904 = ORIENTED_EDGE ( 'NONE', *, *, #22371, .T. ) ;
#18905 = AXIS2_PLACEMENT_3D ( 'NONE', #19640, #2086, #18280 ) ;
#18906 = EDGE_CURVE ( 'NONE', #12945, #7407, #20998, .T. ) ;
#18907 = B_SPLINE_CURVE_WITH_KNOTS ( 'NONE', 3,
 ( #21562, #5837, #18164, #12867, #2417, #16443 ),
 .UNSPECIFIED., .F., .F.,
 ( 4, 2, 4 ),
 ( 2.380730968161660289E-07, 0.002629065763328376944, 0.005257893453559938333 ),
 .UNSPECIFIED. ) ;
#18908 = PRODUCT_DEFINITION_SHAPE ( 'NONE', 'NONE',  #22694 ) ;
#18909 = CARTESIAN_POINT ( 'NONE',  ( -68.71681667565957241, 71.82428002877158235, 85.89527988174788220 ) ) ;
#18910 = EDGE_CURVE ( 'NONE', #3676, #5640, #20659, .T. ) ;
#18911 = PRODUCT_DEFINITION_CONTEXT ( 'detailed design', #21130, 'design' ) ;
#18912 = DIRECTION ( 'NONE',  ( 0.01292414190464131335, 0.000000000000000000, 0.9999164797902017066 ) ) ;
#18913 = CARTESIAN_POINT ( 'NONE',  ( 19.17420491522518944, 147.8948958764534325, 276.8099206193942905 ) ) ;
#18914 = EDGE_LOOP ( 'NONE', ( #20301, #2268, #20386, #19242 ) ) ;
#18915 = DIRECTION ( 'NONE',  ( -0.3101392564284312647, -0.9506461370142480494, 0.009250070373107143265 ) ) ;
#18916 = DIRECTION ( 'NONE',  ( 0.9999164797902015955, 2.045145117964614424E-15, -0.01292414190464167591 ) ) ;
#18917 = ORIENTED_EDGE ( 'NONE', *, *, #21191, .F. ) ;
#18918 = FACE_OUTER_BOUND ( 'NONE', #7263, .T. ) ;
#18919 = CIRCLE ( 'NONE', #4974, 20.50000000000000355 ) ;
#18920 = EDGE_CURVE ( 'NONE', #19445, #7377, #4116, .T. ) ;
#18921 = ORIENTED_EDGE ( 'NONE', *, *, #2638, .T. ) ;
#18922 = CARTESIAN_POINT ( 'NONE',  ( -0.4135725409484799497, 72.00000000000000000, -31.99732735328654343 ) ) ;
#18923 = EDGE_CURVE ( 'NONE', #17586, #1365, #5222, .T. ) ;
#18924 = FACE_OUTER_BOUND ( 'NONE', #1355, .T. ) ;
#18925 = CARTESIAN_POINT ( 'NONE',  ( 10.31485404155361074, 143.0931589593379840, 274.9343155965042342 ) ) ;
#18926 = CARTESIAN_POINT ( 'NONE',  ( -12.01334469841415498, 182.4622809814591449, 320.5389699414921552 ) ) ;
#18927 = CARTESIAN_POINT ( 'NONE',  ( -3.295963053184979508, 157.3739774023628968, 323.7429031424746881 ) ) ;
#18928 = DIRECTION ( 'NONE',  ( -7.125109674161246868E-05, 0.9999848031710253382, -0.005512562950850155054 ) ) ;
#18929 = DIRECTION ( 'NONE',  ( 7.125109674160258889E-05, -0.9999848031710252272, 0.005512562950849897447 ) ) ;
#18930 = EDGE_CURVE ( 'NONE', #1264, #5811, #22093, .T. ) ;
#18931 = EDGE_LOOP ( 'NONE', ( #16933, #5190, #7037, #16020 ) ) ;
#18932 = CARTESIAN_POINT ( 'NONE',  ( -39.40254987707579915, 92.58578643762696458, 84.93055112583746791 ) ) ;
#18933 = DIRECTION ( 'NONE',  ( -0.01292394549866737741, -0.005513023399721125699, -0.9999012842304693116 ) ) ;
#18934 = LINE ( 'NONE', #3191, #6702 ) ;
#18935 = DIRECTION ( 'NONE',  ( -0.8981428216242088869, 0.000000000000000000, -0.4397038457472307593 ) ) ;
#18936 = CARTESIAN_POINT ( 'NONE',  ( 48.31072223536580879, 166.8507685304811048, 256.0170097695140043 ) ) ;
#18937 = ORIENTED_EDGE ( 'NONE', *, *, #4591, .F. ) ;
#18938 = FACE_OUTER_BOUND ( 'NONE', #7456, .T. ) ;
#18939 = LINE ( 'NONE', #22360, #20679 ) ;
#18940 = EDGE_LOOP ( 'NONE', ( #1732, #21032, #21149, #13052 ) ) ;
#18941 = CARTESIAN_POINT ( 'NONE',  ( 51.64825477779187679, 109.2957511350118409, -44.83726143016509269 ) ) ;
#18942 = VERTEX_POINT ( 'NONE', #5364 ) ;
#18943 = B_SPLINE_CURVE_WITH_KNOTS ( 'NONE', 3,
 ( #19873, #14633, #14868, #12901, #18519, #2779 ),
 .UNSPECIFIED., .F., .F.,
 ( 4, 2, 4 ),
 ( 0.009270618776430233909, 0.01189894710419334839, 0.01452727543195646287 ),
 .UNSPECIFIED. ) ;
#18944 = FACE_OUTER_BOUND ( 'NONE', #12083, .T. ) ;
#18945 = CARTESIAN_POINT ( 'NONE',  ( 51.64670511766545502, 84.99999999999997158, -27.66980033337678790 ) ) ;
#18946 = DIRECTION ( 'NONE',  ( 0.006837993415046672921, 0.8485676841065771248, 0.5290426517172845955 ) ) ;
#18947 = ORIENTED_EDGE ( 'NONE', *, *, #16695, .F. ) ;
#18948 = ADVANCED_FACE ( 'NONE', ( #16089 ), #20274, .T. ) ;
#18949 = DIRECTION ( 'NONE',  ( -0.1136178953597573593, 0.9935164314186355483, -0.004009283626633517415 ) ) ;
#18950 = CARTESIAN_POINT ( 'NONE',  ( 68.71681667565954399, 91.17157287525390075, -85.89527988174788220 ) ) ;
#18951 = EDGE_CURVE ( 'NONE', #9416, #3659, #21220, .T. ) ;
#18952 = EDGE_LOOP ( 'NONE', ( #17620, #22501, #14510, #19422 ) ) ;
#18953 = CARTESIAN_POINT ( 'NONE',  ( 48.37538072690065150, 95.13735778864688086, -44.95265272237791976 ) ) ;
#18954 = DIRECTION ( 'NONE',  ( -0.9250486434174662875, -0.3795887553195633202, 0.01404934683357507604 ) ) ;
#18955 = ORIENTED_EDGE ( 'NONE', *, *, #7267, .T. ) ;
#18956 = CARTESIAN_POINT ( 'NONE',  ( 90.14709923383520618, 71.28417594712831828, -63.03576606772374902 ) ) ;
#18957 = CARTESIAN_POINT ( 'NONE',  ( -90.14732535998963669, 87.29974025575781127, 51.21605703091586292 ) ) ;
#18958 = EDGE_LOOP ( 'NONE', ( #2447, #12099 ) ) ;
#18959 = ORIENTED_EDGE ( 'NONE', *, *, #19630, .T. ) ;
#18960 = ORIENTED_EDGE ( 'NONE', *, *, #10480, .F. ) ;
#18961 = CARTESIAN_POINT ( 'NONE',  ( -74.66530369357522545, 95.67986229880271765, 80.77815352928402604 ) ) ;
#18962 = DIRECTION ( 'NONE',  ( 0.9909299940865188283, -0.1338359446631172955, -0.01207007604876047212 ) ) ;
#18963 = FACE_OUTER_BOUND ( 'NONE', #5, .T. ) ;
#18964 = DIRECTION ( 'NONE',  ( -5.440186201345738641E-18, -1.000000000000000000, -1.334940939666364181E-17 ) ) ;
#18965 = CARTESIAN_POINT ( 'NONE',  ( 84.08901704884495132, 75.05050884166001879, 2.023140727569861408 ) ) ;
#18966 = DIRECTION ( 'NONE',  ( 2.025474946048326158E-22, -1.000000000000000000, 1.876735158486679638E-22 ) ) ;
#18967 = VECTOR ( 'NONE', #16023, 1000.000000000000227 ) ;
#18968 = CARTESIAN_POINT ( 'NONE',  ( -51.58190103849386787, 189.4920902165459609, -91.52380460646458005 ) ) ;
#18969 = EDGE_LOOP ( 'NONE', ( #12369, #3115, #17424, #18917, #12208 ) ) ;
#18970 = VERTEX_POINT ( 'NONE', #3882 ) ;
#18971 = ORIENTED_EDGE ( 'NONE', *, *, #9799, .T. ) ;
#18972 = DIRECTION ( 'NONE',  ( -0.008205354412248759208, 0.7726059781012496464, -0.6348327927582039232 ) ) ;
#18973 = CARTESIAN_POINT ( 'NONE',  ( -56.89103422957282419, 143.2573102595449654, 47.48611753646095224 ) ) ;
#18974 = DIRECTION ( 'NONE',  ( 0.006837993415046672921, 0.8485676841065771248, 0.5290426517172845955 ) ) ;
#18975 = CARTESIAN_POINT ( 'NONE',  ( -65.90110554552374822, 103.0000000000000000, -69.29678410920486442 ) ) ;
#18976 = EDGE_CURVE ( 'NONE', #10639, #9934, #9280, .T. ) ;
#18977 = CARTESIAN_POINT ( 'NONE',  ( -5.907585137310531032, 144.0910834040820703, 276.2173154596309246 ) ) ;
#18978 = ORIENTED_EDGE ( 'NONE', *, *, #11027, .F. ) ;
#18979 = ADVANCED_FACE ( 'NONE', ( #19613 ), #19892, .T. ) ;
#18980 = CARTESIAN_POINT ( 'NONE',  ( 0.000000000000000000, 0.000000000000000000, 0.000000000000000000 ) ) ;
#18981 = CARTESIAN_POINT ( 'NONE',  ( -1.632550740186649252, 142.7036636415817838, 274.8672572718561469 ) ) ;
#18982 = DIRECTION ( 'NONE',  ( 2.449293598294706414E-16, -0.000000000000000000, 1.000000000000000000 ) ) ;
#18983 = ORIENTED_EDGE ( 'NONE', *, *, #10385, .T. ) ;
#18984 = EDGE_LOOP ( 'NONE', ( #17281, #13794 ) ) ;
#18985 = VERTEX_POINT ( 'NONE', #7104 ) ;
#18986 = AXIS2_PLACEMENT_3D ( 'NONE', #6880, #3786, #19402 ) ;
#18987 = CARTESIAN_POINT ( 'NONE',  ( -20.15201938634779921, 7.270595330592057870, -11.63220634452945390 ) ) ;
#18988 = CIRCLE ( 'NONE', #3236, 8.000000000000003553 ) ;
#18990 = ORIENTED_EDGE ( 'NONE', *, *, #5040, .T. ) ;
#18989 = ORIENTED_EDGE ( 'NONE', *, *, #2832, .F. ) ;
#18991 = CARTESIAN_POINT ( 'NONE',  ( -90.08121473318537653, 71.65624093448303711, 60.24707949207349600 ) ) ;
#18992 = AXIS2_PLACEMENT_3D ( 'NONE', #1687, #20505, #8331 ) ;
#18993 = CARTESIAN_POINT ( 'NONE',  ( -108.2112308668079095, 76.78797451630623527, 19.89137302265076457 ) ) ;
#18994 = DIRECTION ( 'NONE',  ( 0.009760756503427813965, -0.9999378516499565217, 0.005387065077611106687 ) ) ;
#18995 = FACE_OUTER_BOUND ( 'NONE', #11739, .T. ) ;
#18996 = CARTESIAN_POINT ( 'NONE',  ( 161.9999999999998579, 20.00000000000000000, -10.00000000000224176 ) ) ;
#18997 = DIRECTION ( 'NONE',  ( -0.9934404589540162256, -0.1135548637187056842, 0.01346653032743081423 ) ) ;
#18998 = CARTESIAN_POINT ( 'NONE',  ( -44.75576560912451640, 168.6025580852140706, 19.18675944895310082 ) ) ;
#18999 = DIRECTION ( 'NONE',  ( 0.009760756503428037745, -0.9999378516499566327, 0.005387065077611006073 ) ) ;
#19000 = AXIS2_PLACEMENT_3D ( 'NONE', #21626, #4529, #2245 ) ;
#19001 = CYLINDRICAL_SURFACE ( 'NONE', #18004, 5.099999999999994316 ) ;
#19002 = EDGE_CURVE ( 'NONE', #19051, #12157, #8187, .T. ) ;
#19003 = LINE ( 'NONE', #6833, #12512 ) ;
#19004 = DIRECTION ( 'NONE',  ( -0.01292394549866739996, -0.005513023399721131770, -0.9999012842304692006 ) ) ;
#19005 = ORIENTED_EDGE ( 'NONE', *, *, #2199, .T. ) ;
#19006 = CARTESIAN_POINT ( 'NONE',  ( -91.23438425464435397, 78.34087653192912626, -30.69541483481172861 ) ) ;
#19007 = AXIS2_PLACEMENT_3D ( 'NONE', #7953, #2796, #20237 ) ;
#19008 = ORIENTED_EDGE ( 'NONE', *, *, #15975, .F. ) ;
#19009 = VECTOR ( 'NONE', #1316, 1000.000000000000000 ) ;
#19010 = CIRCLE ( 'NONE', #20845, 5.999999999999952038 ) ;
#19011 = DIRECTION ( 'NONE',  ( 0.01292414190464131335, 0.000000000000000000, 0.9999164797902017066 ) ) ;
#19012 = EDGE_CURVE ( 'NONE', #5068, #1879, #4102, .T. ) ;
#19013 = CARTESIAN_POINT ( 'NONE',  ( -88.04457284303852305, 72.00000000000000000, 62.11887076636494953 ) ) ;
#19014 = LINE ( 'NONE', #3276, #12448 ) ;
#19015 = CARTESIAN_POINT ( 'NONE',  ( 11.38205409781506816, 143.4374251742922866, 275.3786240061384092 ) ) ;
#19016 = EDGE_CURVE ( 'NONE', #10791, #16568, #9158, .T. ) ;
#19017 = EDGE_LOOP ( 'NONE', ( #12788, #13299 ) ) ;
#19018 = CARTESIAN_POINT ( 'NONE',  ( 12.53310868402590827, 188.2157523762948870, 320.9566087149508462 ) ) ;
#19019 = ORIENTED_EDGE ( 'NONE', *, *, #22435, .T. ) ;
#19020 = CARTESIAN_POINT ( 'NONE',  ( -154.0000000000000000, 1.999999999999998224, 53.76161406891259986 ) ) ;
#19021 = CIRCLE ( 'NONE', #15029, 95.00000000000001421 ) ;
#19022 = CARTESIAN_POINT ( 'NONE',  ( 109.5818730699487560, 75.33563225513333350, -10.60333173834208687 ) ) ;
#19023 = CARTESIAN_POINT ( 'NONE',  ( 109.7386064778677905, 75.43227853978193309, 7.937952133666850152 ) ) ;
#19024 = AXIS2_PLACEMENT_3D ( 'NONE', #15057, #9655, #6532 ) ;
#19025 = FACE_OUTER_BOUND ( 'NONE', #18089, .T. ) ;
#19026 = ORIENTED_EDGE ( 'NONE', *, *, #14135, .T. ) ;
#19027 = EDGE_CURVE ( 'NONE', #16423, #4610, #7062, .T. ) ;
#19028 = DIRECTION ( 'NONE',  ( -0.1136178953597579422, 0.9935164314186355483, -0.004009283626633659663 ) ) ;
#19029 = EDGE_CURVE ( 'NONE', #2627, #15447, #17698, .T. ) ;
#19030 = VERTEX_POINT ( 'NONE', #14366 ) ;
#19031 = DIRECTION ( 'NONE',  ( 0.3101392564284308762, 0.9506461370142480494, -0.009250070373106863975 ) ) ;
#19032 = CARTESIAN_POINT ( 'NONE',  ( 39.33558597195864337, 105.5072037373731604, 91.67806775769213345 ) ) ;
#19033 = CARTESIAN_POINT ( 'NONE',  ( -1.163172771417704698, 44.99899999999999523, -89.99248318111816047 ) ) ;
#19034 = FACE_OUTER_BOUND ( 'NONE', #12017, .T. ) ;
#19035 = AXIS2_PLACEMENT_3D ( 'NONE', #2380, #19924, #11106 ) ;
#19036 = CYLINDRICAL_SURFACE ( 'NONE', #12818, 2.000000000000001332 ) ;
#19037 = DIRECTION ( 'NONE',  ( -0.7944560844389300103, 0.000000000000000000, -0.6073216033519338586 ) ) ;
#19038 = ADVANCED_FACE ( 'NONE', ( #11130 ), #17817, .T. ) ;
#19039 = VECTOR ( 'NONE', #468, 1000.000000000000000 ) ;
#19040 = CARTESIAN_POINT ( 'NONE',  ( 21.01742933042251948, 97.26594046717957553, 78.58734125711376350 ) ) ;
#19041 = EDGE_CURVE ( 'NONE', #309, #3054, #1940, .T. ) ;
#19042 = VERTEX_POINT ( 'NONE', #330 ) ;
#19043 = CARTESIAN_POINT ( 'NONE',  ( -50.56656660976580753, 108.3817487785542397, -43.51107281728322107 ) ) ;
#19044 = EDGE_CURVE ( 'NONE', #11923, #7115, #17730, .T. ) ;
#19045 = CARTESIAN_POINT ( 'NONE',  ( 11.20671232108558257, 174.3736497049977174, 324.1290499907220237 ) ) ;
#19046 = CARTESIAN_POINT ( 'NONE',  ( -93.18417523045798134, 77.12912189496638860, -26.79791266334240873 ) ) ;
#19047 = DIRECTION ( 'NONE',  ( 0.1136178953597573732, -0.9935164314186356593, 0.004009283626633518283 ) ) ;
#19048 = VERTEX_POINT ( 'NONE', #21335 ) ;
#19049 = CARTESIAN_POINT ( 'NONE',  ( 7.145902869757795983, 81.99999999999998579, -93.45069977196735067 ) ) ;
#19050 = CARTESIAN_POINT ( 'NONE',  ( -59.30749807291185505, 114.2358014486931808, 170.6782526301398661 ) ) ;
#19051 = VERTEX_POINT ( 'NONE', #2282 ) ;
#19052 = DIRECTION ( 'NONE',  ( -7.125109674161230605E-05, 0.9999848031710253382, -0.005512562950850140309 ) ) ;
#19053 = ORIENTED_EDGE ( 'NONE', *, *, #4476, .F. ) ;
#19054 = CARTESIAN_POINT ( 'NONE',  ( 106.2089377515399065, 77.12912189496647386, 28.62973177816241588 ) ) ;
#19055 = PLANE ( 'NONE',  #11293 ) ;
#19056 = CARTESIAN_POINT ( 'NONE',  ( 49.99582398951007889, 170.0000000000000284, -0.6462070952321007367 ) ) ;
#19057 = AXIS2_PLACEMENT_3D ( 'NONE', #5827, #21125, #18158 ) ;
#19058 = B_SPLINE_CURVE_WITH_KNOTS ( 'NONE', 3,
 ( #12250, #4878, #1457, #10407, #17426, #13639, #15371, #10077, #8435, #22439 ),
 .UNSPECIFIED., .F., .F.,
 ( 4, 2, 2, 2, 4 ),
 ( -8.944271960021110598E-06, 0.0009933947872009813579, 0.001995733846361983505, 0.002998072905522986085, 0.004000411964683988665 ),
 .UNSPECIFIED. ) ;
#19059 = ADVANCED_FACE ( 'NONE', ( #2051 ), #1944, .T. ) ;
#19060 = CIRCLE ( 'NONE', #12832, 2.000000000000001776 ) ;
#19061 = EDGE_CURVE ( 'NONE', #16549, #5690, #7449, .T. ) ;
#19062 = CARTESIAN_POINT ( 'NONE',  ( -1.886058359258391270, 327.1149038793577120, 318.8066435240484111 ) ) ;
#19063 = DIRECTION ( 'NONE',  ( -0.01292394549866738608, -0.005513023399720699824, -0.9999012842304692006 ) ) ;
#19064 = ORIENTED_EDGE ( 'NONE', *, *, #1683, .F. ) ;
#19065 = CARTESIAN_POINT ( 'NONE',  ( 21.94165880485012110, 168.7756884006963389, 313.8512965718784926 ) ) ;
#19066 = AXIS2_PLACEMENT_3D ( 'NONE', #1374, #8348, #3292 ) ;
#19067 = ORIENTED_EDGE ( 'NONE', *, *, #20291, .T. ) ;
#19068 = CARTESIAN_POINT ( 'NONE',  ( 91.85265939091880227, 69.99999999999998579, -60.52463885842053060 ) ) ;
#19069 = CARTESIAN_POINT ( 'NONE',  ( -90.04282273172685791, 88.64429409703403451, 52.59290563217275150 ) ) ;
#19070 = LINE ( 'NONE', #10364, #11900 ) ;
#19071 = AXIS2_PLACEMENT_3D ( 'NONE', #17645, #21182, #10860 ) ;
#19072 = ORIENTED_EDGE ( 'NONE', *, *, #22371, .F. ) ;
#19073 = VECTOR ( 'NONE', #11302, 1000.000000000000000 ) ;
#19074 = EDGE_CURVE ( 'NONE', #552, #8312, #13694, .T. ) ;
#19075 = VERTEX_POINT ( 'NONE', #677 ) ;
#19076 = CARTESIAN_POINT ( 'NONE',  ( -9.638276707334691551, 184.4631002042323757, 323.1821100297731846 ) ) ;
#19077 = CARTESIAN_POINT ( 'NONE',  ( 49.42284594772163331, 139.7551263635817236, -44.97643735496247785 ) ) ;
#19078 = CARTESIAN_POINT ( 'NONE',  ( -1.745728752920420179, 86.14745084375783790, -74.98370060827653560 ) ) ;
#19079 = AXIS2_PLACEMENT_3D ( 'NONE', #9482, #12959, #7767 ) ;
#19080 = SURFACE_STYLE_FILL_AREA ( #20574 ) ;
#19081 = CARTESIAN_POINT ( 'NONE',  ( 85.06848091764891251, 75.00179123396263492, -0.4306469408276333843 ) ) ;
#19082 = CARTESIAN_POINT ( 'NONE',  ( -11.19153202869804353, 137.5572120012638777, 101.3144779797563189 ) ) ;
#19083 = VERTEX_POINT ( 'NONE', #4321 ) ;
#19084 = TOROIDAL_SURFACE ( 'NONE', #12130, 4.000000000000000000, 2.000000000000000000 ) ;
#19085 = EDGE_LOOP ( 'NONE', ( #20109, #22214, #4241, #970, #2237, #12202 ) ) ;
#19086 = CARTESIAN_POINT ( 'NONE',  ( -11.34375974262850129, 185.6357169915080760, 278.3389279131694138 ) ) ;
#19087 = CARTESIAN_POINT ( 'NONE',  ( 9.674709713264089326E-15, 0.000000000000000000, 78.99999999999998579 ) ) ;
#19088 = DIRECTION ( 'NONE',  ( 7.125109674364536131E-05, -0.9999848031710253382, 0.005512562950849705760 ) ) ;
#19089 = CARTESIAN_POINT ( 'NONE',  ( -59.48801398013453223, 114.2839059398627484, 164.5936811294757263 ) ) ;
#19090 = CARTESIAN_POINT ( 'NONE',  ( -2.775788928915473797, 142.9626891742539669, 275.1092189909475678 ) ) ;
#19091 = EDGE_CURVE ( 'NONE', #18552, #9134, #3404, .T. ) ;
#19092 = DIRECTION ( 'NONE',  ( 1.000000000000000000, 0.000000000000000000, 0.000000000000000000 ) ) ;
#19093 = AXIS2_PLACEMENT_3D ( 'NONE', #14414, #20928, #12681 ) ;
#19094 = CARTESIAN_POINT ( 'NONE',  ( 1.166418432474939088E-15, 1.999999999999998224, 7.999999999999994671 ) ) ;
#19095 = AXIS2_PLACEMENT_3D ( 'NONE', #19162, #5604, #7002 ) ;
#19096 =( BOUNDED_CURVE ( )  B_SPLINE_CURVE ( 3, ( #21613, #14898, #4174, #629 ),
 .UNSPECIFIED., .F., .T. ) 
 B_SPLINE_CURVE_WITH_KNOTS ( ( 4, 4 ),
 ( 0.6960171423055203643, 0.8501495483016222598 ),
 .UNSPECIFIED. ) 
 CURVE ( )  GEOMETRIC_REPRESENTATION_ITEM ( )  RATIONAL_B_SPLINE_CURVE ( ( 1.000000000000000000, 0.9980212464270939998, 0.9980212464270939998, 1.000000000000000000 ) ) 
 REPRESENTATION_ITEM ( '' )  );
#19097 = DIRECTION ( 'NONE',  ( 7.125109674403838460E-05, -0.9999848031710254492, 0.005512562950847868688 ) ) ;
#19098 = EDGE_LOOP ( 'NONE', ( #9731, #12372, #12691, #8071 ) ) ;
#19099 = ORIENTED_EDGE ( 'NONE', *, *, #1952, .T. ) ;
#19100 = UNCERTAINTY_MEASURE_WITH_UNIT (LENGTH_MEASURE( 1.000000000000000082E-05 ), #2464, 'distance_accuracy_value', 'NONE');
#19101 = CARTESIAN_POINT ( 'NONE',  ( -93.23587179807654479, 34.61572286322119396, -30.79757858250321689 ) ) ;
#19102 = ORIENTED_EDGE ( 'NONE', *, *, #1431, .T. ) ;
#19103 = EDGE_CURVE ( 'NONE', #11611, #6360, #910, .T. ) ;
#19104 = CARTESIAN_POINT ( 'NONE',  ( 19.46476238196024866, 175.6255473142593360, 113.2095803124133511 ) ) ;
#19105 = PLANE ( 'NONE',  #20257 ) ;
#19106 = EDGE_CURVE ( 'NONE', #6085, #15577, #7807, .T. ) ;
#19107 = FACE_OUTER_BOUND ( 'NONE', #10376, .T. ) ;
#19108 = AXIS2_PLACEMENT_3D ( 'NONE', #5562, #7284, #7181 ) ;
#19109 = CARTESIAN_POINT ( 'NONE',  ( -93.58499681124557412, 69.99999999999998579, -57.80872228166919058 ) ) ;
#19110 = AXIS2_PLACEMENT_3D ( 'NONE', #18611, #20335, #2875 ) ;
#19111 = ORIENTED_EDGE ( 'NONE', *, *, #4984, .T. ) ;
#19112 = PLANE ( 'NONE',  #22467 ) ;
#19113 = AXIS2_PLACEMENT_3D ( 'NONE', #15235, #6481, #5065 ) ;
#19114 = FACE_OUTER_BOUND ( 'NONE', #14376, .T. ) ;
#19115 = CARTESIAN_POINT ( 'NONE',  ( 84.78539177974978713, 105.0000000000000000, 70.08164767436862519 ) ) ;
#19116 = FACE_OUTER_BOUND ( 'NONE', #2083, .T. ) ;
#19117 = CIRCLE ( 'NONE', #7021, 5.699999999999990408 ) ;
#19118 = DIRECTION ( 'NONE',  ( -0.01292394549866738782, -0.005513023399720468239, -0.9999012842304692006 ) ) ;
#19119 = CARTESIAN_POINT ( 'NONE',  ( 90.02055463237803679, 34.61572286322119396, -63.21629334023821656 ) ) ;
#19120 = VERTEX_POINT ( 'NONE', #15165 ) ;
#19121 = CARTESIAN_POINT ( 'NONE',  ( -89.24560213809745335, 80.14548850073745712, -29.69112557292186949 ) ) ;
#19122 = VERTEX_POINT ( 'NONE', #21996 ) ;
#19123 = AXIS2_PLACEMENT_3D ( 'NONE', #5415, #381, #12688 ) ;
#19124 = AXIS2_PLACEMENT_3D ( 'NONE', #4514, #4847, #15239 ) ;
#19125 = AXIS2_PLACEMENT_3D ( 'NONE', #18387, #2766, #13017 ) ;
#19126 = DIRECTION ( 'NONE',  ( -2.025474946048326393E-22, 1.000000000000000000, -1.876735158486679873E-22 ) ) ;
#19127 = FACE_BOUND ( 'NONE', #8143, .T. ) ;
#19128 = CARTESIAN_POINT ( 'NONE',  ( 21.10182743699991903, 147.3736716370421789, 276.4577479339097863 ) ) ;
#19129 = ORIENTED_EDGE ( 'NONE', *, *, #1387, .T. ) ;
#19130 = CARTESIAN_POINT ( 'NONE',  ( -13.98112707844397562, 325.7531995422979207, 324.1294444254230598 ) ) ;
#19131 = ORIENTED_EDGE ( 'NONE', *, *, #5330, .F. ) ;
#19132 = AXIS2_PLACEMENT_3D ( 'NONE', #12416, #19403, #14029 ) ;
#19133 = CARTESIAN_POINT ( 'NONE',  ( 13.76243855136152838, 137.5384677217048193, 97.59171006575670049 ) ) ;
#19134 = AXIS2_PLACEMENT_3D ( 'NONE', #18149, #2399, #9390 ) ;
#19135 = VECTOR ( 'NONE', #18236, 1000.000000000000114 ) ;
#19136 = CARTESIAN_POINT ( 'NONE',  ( -4.029718584172675477, 174.3038068289426690, 299.6566739225319225 ) ) ;
#19137 = EDGE_LOOP ( 'NONE', ( #22020, #9241, #12434 ) ) ;
#19138 = DIRECTION ( 'NONE',  ( 0.01292394549866738782, 0.005513023399720468239, 0.9999012842304692006 ) ) ;
#19139 = DIRECTION ( 'NONE',  ( 7.125109674160325297E-05, -0.9999848031710252272, 0.005512562950849327591 ) ) ;
#19140 = ORIENTED_EDGE ( 'NONE', *, *, #13196, .F. ) ;
#19141 = CARTESIAN_POINT ( 'NONE',  ( 41.58451242677340076, 92.58578643762696458, 83.88377541325534992 ) ) ;
#19142 = EDGE_CURVE ( 'NONE', #4735, #6191, #13200, .T. ) ;
#19143 = EDGE_LOOP ( 'NONE', ( #4064, #19249, #15753, #18382 ) ) ;
#19144 = CARTESIAN_POINT ( 'NONE',  ( -92.28892611776123545, 77.12912189496636017, 31.19536062043662739 ) ) ;
#19145 = AXIS2_PLACEMENT_3D ( 'NONE', #9999, #4923, #15635 ) ;
#19146 = CARTESIAN_POINT ( 'NONE',  ( 49.00068018611270304, 169.5754971982215125, -77.63860598097826937 ) ) ;
#19147 = CARTESIAN_POINT ( 'NONE',  ( 161.9999999999998579, 20.00000000000000000, 10.00000000000220091 ) ) ;
#19148 = CARTESIAN_POINT ( 'NONE',  ( 16.76385840201456290, 185.2028283229317651, 306.7113249663256056 ) ) ;
#19149 = CARTESIAN_POINT ( 'NONE',  ( 9.142505149400548703, 81.99999999999998579, -88.65345271381772818 ) ) ;
#19150 = DIRECTION ( 'NONE',  ( 7.125109674364534776E-05, -0.9999848031710252272, 0.005512562950849704893 ) ) ;
#19151 = CIRCLE ( 'NONE', #82, 2.000000000000001332 ) ;
#19152 = CARTESIAN_POINT ( 'NONE',  ( -12.64688860274155324, 109.6831087301383860, 124.2482791415423691 ) ) ;
#19153 = AXIS2_PLACEMENT_3D ( 'NONE', #19553, #10716, #30 ) ;
#19154 = DIRECTION ( 'NONE',  ( 0.9999164797902017066, 0.000000000000000000, -0.01292414190463751951 ) ) ;
#19155 = ITEM_DEFINED_TRANSFORMATION ( 'NONE', 'NONE', #3680,  #6292 ) ;
#19156 = CARTESIAN_POINT ( 'NONE',  ( 37.52478479852118909, 92.78536193179812130, 82.71535724525615763 ) ) ;
#19157 = EDGE_CURVE ( 'NONE', #9612, #22002, #21658, .T. ) ;
#19158 = ORIENTED_EDGE ( 'NONE', *, *, #16005, .F. ) ;
#19159 = EDGE_CURVE ( 'NONE', #7061, #5236, #10010, .T. ) ;
#19160 = DIRECTION ( 'NONE',  ( 0.01035335185279138807, 0.005513005182356417802, 0.9999312050732649393 ) ) ;
#19161 = CARTESIAN_POINT ( 'NONE',  ( -158.3970384574724335, 18.00000000000000355, -62.74304228515459414 ) ) ;
#19162 = CARTESIAN_POINT ( 'NONE',  ( 157.5176307659771169, 2.000000000000000000, 60.94675664190834397 ) ) ;
#19163 = AXIS2_PLACEMENT_3D ( 'NONE', #3193, #11845, #18834 ) ;
#19164 = DIRECTION ( 'NONE',  ( 0.01292394549866738782, 0.005513023399720468239, 0.9999012842304692006 ) ) ;
#19165 = ORIENTED_EDGE ( 'NONE', *, *, #14926, .T. ) ;
#19166 = FACE_OUTER_BOUND ( 'NONE', #14462, .T. ) ;
#19167 = LINE ( 'NONE', #117, #12898 ) ;
#19168 = ORIENTED_EDGE ( 'NONE', *, *, #7695, .T. ) ;
#19169 = CARTESIAN_POINT ( 'NONE',  ( 50.83832527469255780, 109.9515020747574852, -44.83040843917926566 ) ) ;
#19170 = ORIENTED_EDGE ( 'NONE', *, *, #3184, .F. ) ;
#19171 =( LENGTH_UNIT ( ) NAMED_UNIT ( * ) SI_UNIT ( .MILLI., .METRE. ) );
#19172 = CARTESIAN_POINT ( 'NONE',  ( 106.7230861007157472, 79.13476608364855736, 26.64972274501352700 ) ) ;
#19173 = DIRECTION ( 'NONE',  ( 0.1296504907605108559, 0.005475273188901296634, 0.9915446392518419971 ) ) ;
#19174 = DIRECTION ( 'NONE',  ( 0.01292394549866738782, 0.005513023399720468239, 0.9999012842304692006 ) ) ;
#19175 = AXIS2_PLACEMENT_3D ( 'NONE', #22447, #20851, #6737 ) ;
#19176 = TOROIDAL_SURFACE ( 'NONE', #9276, 118.0000000000000000, 2.000000000000000000 ) ;
#19177 = EDGE_CURVE ( 'NONE', #10848, #5715, #104, .T. ) ;
#19178 = DIRECTION ( 'NONE',  ( -0.9999164797902015955, -6.965998958219364448E-18, 0.01292414190464157182 ) ) ;
#19179 = CARTESIAN_POINT ( 'NONE',  ( -158.3970384574724051, 20.00000000000000000, 62.74304228515463677 ) ) ;
#19180 = EDGE_CURVE ( 'NONE', #10707, #6260, #16430, .T. ) ;
#19181 = ORIENTED_EDGE ( 'NONE', *, *, #22537, .T. ) ;
#19182 = CARTESIAN_POINT ( 'NONE',  ( 21.46898066623532841, 168.7138791228462367, 311.9297967271122047 ) ) ;
#19183 = EDGE_CURVE ( 'NONE', #11089, #12054, #855, .T. ) ;
#19184 = CARTESIAN_POINT ( 'NONE',  ( 16.46024795975520760, 187.9730162318629425, 275.8249587968540482 ) ) ;
#19185 = ORIENTED_EDGE ( 'NONE', *, *, #15855, .F. ) ;
#19186 = CIRCLE ( 'NONE', #6367, 24.99999999999998224 ) ;
#19187 = CARTESIAN_POINT ( 'NONE',  ( 90.64004788018706904, 70.55772556090482794, -62.32501834406217256 ) ) ;
#19188 = CARTESIAN_POINT ( 'NONE',  ( -90.04229551167981072, 87.63269930271252406, 51.01256596538104304 ) ) ;
#19189 = CARTESIAN_POINT ( 'NONE',  ( -63.99205529224568068, 99.43075776215394512, 78.40283286226222970 ) ) ;
#19190 = CIRCLE ( 'NONE', #18470, 5.100000000000004974 ) ;
#19192 = EDGE_LOOP ( 'NONE', ( #19838, #6208 ) ) ;
#19191 = ORIENTED_EDGE ( 'NONE', *, *, #2807, .T. ) ;
#19193 = AXIS2_PLACEMENT_3D ( 'NONE', #22282, #16721, #18747 ) ;
#19194 = EDGE_CURVE ( 'NONE', #6995, #2627, #8531, .T. ) ;
#19195 = VERTEX_POINT ( 'NONE', #9849 ) ;
#19196 = CARTESIAN_POINT ( 'NONE',  ( -73.09270779449821021, 95.74768611921976458, 82.20384009048147789 ) ) ;
#19197 = DIRECTION ( 'NONE',  ( -0.9999164797902015955, -6.965998958219364448E-18, 0.01292414190464157182 ) ) ;
#19198 = PRESENTATION_STYLE_ASSIGNMENT (( #15663 ) ) ;
#19199 = CARTESIAN_POINT ( 'NONE',  ( 84.59857130917060886, 75.02669947309938436, 1.163726430838213810 ) ) ;
#19200 = DIRECTION ( 'NONE',  ( 0.9934404589540162256, 0.1135548637187059617, -0.01346653032742970747 ) ) ;
#19201 = ORIENTED_EDGE ( 'NONE', *, *, #110, .F. ) ;
#19202 = ORIENTED_EDGE ( 'NONE', *, *, #6832, .F. ) ;
#19203 = LINE ( 'NONE', #19087, #10424 ) ;
#19204 = AXIS2_PLACEMENT_3D ( 'NONE', #22209, #20383, #1112 ) ;
#19205 = CARTESIAN_POINT ( 'NONE',  ( -75.43851917653510952, 75.02636992936612614, -1.284289157548322624 ) ) ;
#19206 = B_SPLINE_CURVE_WITH_KNOTS ( 'NONE', 3,
 ( #4743, #7976, #15251, #18993, #4863, #22204, #6497, #21967, #13291, #11666, #1107, #18885, #4532, #1338 ),
 .UNSPECIFIED., .F., .F.,
 ( 4, 2, 2, 2, 2, 2, 4 ),
 ( 0.05403846203490995925, 0.06102746434071378012, 0.06801646664651760099, 0.08199447125812525661, 0.08898347356392907748, 0.09597247586973289835, 0.1099504804813405401 ),
 .UNSPECIFIED. ) ;
#19207 = CARTESIAN_POINT ( 'NONE',  ( -13.77044500111245107, 164.6916052361225979, 313.8339224003136678 ) ) ;
#19208 = CARTESIAN_POINT ( 'NONE',  ( -105.5454984634618114, 78.31265485325657494, 30.98643060412755901 ) ) ;
#19209 = VERTEX_POINT ( 'NONE', #4215 ) ;
#19210 = VECTOR ( 'NONE', #21367, 999.9999999999998863 ) ;
#19211 = CARTESIAN_POINT ( 'NONE',  ( -35.95309506732429128, 93.50464841319750064, -82.03286182426641915 ) ) ;
#19212 = AXIS2_PLACEMENT_3D ( 'NONE', #13256, #6863, #20233 ) ;
#19213 = EDGE_CURVE ( 'NONE', #15796, #15089, #7790, .T. ) ;
#19214 = DIRECTION ( 'NONE',  ( 0.9909299940865186063, -0.1338359446631179339, -0.01207007604875938098 ) ) ;
#19215 = ORIENTED_EDGE ( 'NONE', *, *, #17520, .T. ) ;
#19216 = ORIENTED_EDGE ( 'NONE', *, *, #10783, .F. ) ;
#19217 = CARTESIAN_POINT ( 'NONE',  ( 59.61792454239376582, 143.9050905090123820, 163.4882421145073010 ) ) ;
#19218 = AXIS2_PLACEMENT_3D ( 'NONE', #10709, #17500, #22508 ) ;
#19220 = VERTEX_POINT ( 'NONE', #18249 ) ;
#19219 = ORIENTED_EDGE ( 'NONE', *, *, #2949, .F. ) ;
#19221 = EDGE_CURVE ( 'NONE', #21319, #21410, #15040, .T. ) ;
#19222 = FACE_OUTER_BOUND ( 'NONE', #20259, .T. ) ;
#19223 = CARTESIAN_POINT ( 'NONE',  ( -90.66884163116230866, 70.40480925447369032, 62.28309067965741974 ) ) ;
#19224 = VECTOR ( 'NONE', #83, 1000.000000000000000 ) ;
#19225 = AXIS2_PLACEMENT_3D ( 'NONE', #1332, #20479, #10391 ) ;
#19226 = DIRECTION ( 'NONE',  ( 5.440186201345785633E-18, 1.000000000000000000, 1.334940939666367878E-17 ) ) ;
#19227 = DIRECTION ( 'NONE',  ( 0.01292414190463136471, 0.000000000000000000, 0.9999164797902019286 ) ) ;
#19228 = VERTEX_POINT ( 'NONE', #18581 ) ;
#19229 = CARTESIAN_POINT ( 'NONE',  ( -64.02946135753127521, 99.82858438784199961, 75.50879615180311077 ) ) ;
#19230 = DIRECTION ( 'NONE',  ( -0.01292394549866738782, -0.005513023399720700692, -0.9999012842304693116 ) ) ;
#19231 = CARTESIAN_POINT ( 'NONE',  ( 11.77922689329016848, 187.8031667290258042, 307.7652408209249870 ) ) ;
#19232 = LINE ( 'NONE', #56, #4917 ) ;
#19233 = CARTESIAN_POINT ( 'NONE',  ( 45.33957475275741444, 176.1465482961944815, 25.98145272924774218 ) ) ;
#19234 = VERTEX_POINT ( 'NONE', #16540 ) ;
#19235 =( BOUNDED_SURFACE ( )  B_SPLINE_SURFACE ( 3, 2, ( 
 ( #16765, #1013, #2842 ),
 ( #16870, #2948, #10304 ),
 ( #19128, #15277, #15716 ),
 ( #20968, #18913, #22225 ),
 ( #17101, #3169, #13978 ),
 ( #22331, #8668, #13650 ),
 ( #1362, #11690, #6843 ),
 ( #17437, #6955, #10420 ),
 ( #1694, #15603, #3407 ),
 ( #16997, #13535, #5107 ),
 ( #18807, #6626, #8338 ),
 ( #6517, #19015, #22659 ),
 ( #15382, #10089, #3277 ),
 ( #18683, #9969, #1260 ) ),
 .UNSPECIFIED., .F., .F., .T. ) 
 B_SPLINE_SURFACE_WITH_KNOTS ( ( 4, 2, 2, 2, 2, 2, 4 ),
 ( 3, 3 ),
 ( 3.903127820947815962E-18, 0.001878086432925129287, 0.003756172865850254672, 0.005634259298775380273, 0.007512345731700505874, 0.01126851859755075708, 0.01502469146340100828 ),
 ( 0.000000000000000000, 1.000000000000000000 ),
 .UNSPECIFIED. ) 
 GEOMETRIC_REPRESENTATION_ITEM ( )  RATIONAL_B_SPLINE_SURFACE ( (
 ( 1.000000000000000000, 0.7193398003386550776, 1.000000000000000000),
 ( 1.000000000000000000, 0.7439100388534258812, 1.000000000000000000),
 ( 1.000000000000000000, 0.7665383218973651491, 1.000000000000000000),
 ( 1.000000000000000000, 0.8084046970485163630, 1.000000000000000000),
 ( 1.000000000000000000, 0.8276426232566694852, 1.000000000000000000),
 ( 1.000000000000000000, 0.8630029158313429205, 1.000000000000000000),
 ( 1.000000000000000000, 0.8791524022210245315, 1.000000000000000000),
 ( 1.000000000000000000, 0.9083399791590486272, 1.000000000000000000),
 ( 1.000000000000000000, 0.9212515500161249093, 1.000000000000000000),
 ( 1.000000000000000000, 0.9553996440820913261, 1.000000000000000000),
 ( 1.000000000000000000, 0.9720881558712876069, 1.000000000000000000),
 ( 1.000000000000000000, 0.9943940623859978123, 1.000000000000000000),
 ( 1.000000000000000000, 0.9999834998407445275, 1.000000000000000000),
 ( 1.000000000000000000, 1.000000000000000000, 1.000000000000000000) ) ) 
 REPRESENTATION_ITEM ( '' )  SURFACE ( )  );
#19236 = DIRECTION ( 'NONE',  ( 7.125109674364534776E-05, -0.9999848031710252272, 0.005512562950849704893 ) ) ;
#19237 = AXIS2_PLACEMENT_3D ( 'NONE', #19288, #8603, #6879 ) ;
#19238 = EDGE_CURVE ( 'NONE', #6364, #10233, #11487, .T. ) ;
#19239 = CARTESIAN_POINT ( 'NONE',  ( -39.42082737383935154, 69.99999999999998579, 83.51645567887779009 ) ) ;
#19240 = CARTESIAN_POINT ( 'NONE',  ( -37.99233741293296163, 107.0009574002254453, 0.8384088582799177347 ) ) ;
#19241 = EDGE_CURVE ( 'NONE', #16738, #19195, #7664, .T. ) ;
#19242 = ORIENTED_EDGE ( 'NONE', *, *, #16045, .F. ) ;
#19243 = CARTESIAN_POINT ( 'NONE',  ( -92.25740333814806604, 79.89798572913885266, -28.97539206162185366 ) ) ;
#19244 = ORIENTED_EDGE ( 'NONE', *, *, #4636, .T. ) ;
#19245 = CIRCLE ( 'NONE', #16347, 3.047499999999988329 ) ;
#19246 = DIRECTION ( 'NONE',  ( 0.3101392564284308762, 0.9506461370142480494, -0.009250070373106863975 ) ) ;
#19247 = PRESENTATION_STYLE_ASSIGNMENT (( #2129 ) ) ;
#19248 = PRESENTATION_LAYER_ASSIGNMENT (  '', '', ( #6432 ) ) ;
#19249 = ORIENTED_EDGE ( 'NONE', *, *, #19012, .T. ) ;
#19250 = CARTESIAN_POINT ( 'NONE',  ( -40.54068192821626582, 96.15465585523027414, -41.57304724140053764 ) ) ;
#19251 = DIRECTION ( 'NONE',  ( -0.9999164797902015955, 0.000000000000000000, 0.01292414190464162733 ) ) ;
#19252 = DIRECTION ( 'NONE',  ( -0.01292394549866738261, -0.005513023399719314648, -0.9999012842304692006 ) ) ;
#19253 = DIRECTION ( 'NONE',  ( -0.07120137477123651693, 0.7064205021071690016, 0.7042019869563996837 ) ) ;
#19254 = ORIENTED_EDGE ( 'NONE', *, *, #9033, .T. ) ;
#19255 = CARTESIAN_POINT ( 'NONE',  ( 12.94357278854792170, 190.3382146902982583, 320.8588152455632780 ) ) ;
#19256 = VERTEX_POINT ( 'NONE', #2624 ) ;
#19257 = DIRECTION ( 'NONE',  ( 7.125109674161818785E-05, -0.9999848031710252272, 0.005512562950850596541 ) ) ;
#19258 = DIRECTION ( 'NONE',  ( 0.000000000000000000, -1.000000000000000000, 3.469446951953611033E-15 ) ) ;
#19259 = CARTESIAN_POINT ( 'NONE',  ( -12.58664483627157260, 184.6272112293439704, 320.1917372557448402 ) ) ;
#19260 = CARTESIAN_POINT ( 'NONE',  ( 4.169604791867612015, 166.7785703876306513, 322.5944574396354483 ) ) ;
#19261 = CARTESIAN_POINT ( 'NONE',  ( 39.40254987707581336, 92.58578643762697880, -84.93055112583749633 ) ) ;
#19262 = ORIENTED_EDGE ( 'NONE', *, *, #14703, .F. ) ;
#19263 = CARTESIAN_POINT ( 'NONE',  ( -1.163172771417702700, 81.34441321561124028, -89.99248318111824574 ) ) ;
#19264 = CARTESIAN_POINT ( 'NONE',  ( -90.59090487622916044, 77.87375801460382263, 32.35420311765519585 ) ) ;
#19265 = FACE_OUTER_BOUND ( 'NONE', #18639, .T. ) ;
#19266 = DIRECTION ( 'NONE',  ( 7.125109674161246868E-05, -0.9999848031710252272, 0.005512562950850154186 ) ) ;
#19267 = CIRCLE ( 'NONE', #578, 83.00000000000002842 ) ;
#19268 = CARTESIAN_POINT ( 'NONE',  ( 18.18475692997101589, 184.3587657017563117, 320.8069875086114848 ) ) ;
#19269 = LINE ( 'NONE', #6978, #3458 ) ;
#19270 = FACE_OUTER_BOUND ( 'NONE', #3923, .T. ) ;
#19271 = VERTEX_POINT ( 'NONE', #9637 ) ;
#19272 = CARTESIAN_POINT ( 'NONE',  ( 50.89197640125190958, 108.0238286078847523, 68.68741454989820738 ) ) ;
#19273 = CARTESIAN_POINT ( 'NONE',  ( 41.42315785391630811, 144.7550503794368524, -44.90060703447959156 ) ) ;
#19274 = CARTESIAN_POINT ( 'NONE',  ( 45.44350069997184249, 168.6907664596096765, 34.02200722522287180 ) ) ;
#19275 = LINE ( 'NONE', #3539, #2231 ) ;
#19276 = CARTESIAN_POINT ( 'NONE',  ( 67.23320572660466610, 192.1022009597330680, 17.60971032628828681 ) ) ;
#19277 = DIRECTION ( 'NONE',  ( 0.9999164797902015955, 2.001050586450178695E-22, -0.01292414190464131335 ) ) ;
#19278 = DIRECTION ( 'NONE',  ( -0.01292414190464131335, -1.902755938799530239E-22, -0.9999164797902015955 ) ) ;
#19279 = CARTESIAN_POINT ( 'NONE',  ( 19.43891449096291169, 175.6145212674599065, 111.2097777439524151 ) ) ;
#19280 = CIRCLE ( 'NONE', #7174, 8.000000000000014211 ) ;
#19281 = ORIENTED_EDGE ( 'NONE', *, *, #7734, .T. ) ;
#19282 = DIRECTION ( 'NONE',  ( 0.009760756503428003050, -0.9999378516499564107, 0.005387065077611006073 ) ) ;
#19283 = PRODUCT_DEFINITION_SHAPE ( 'NONE', 'NONE',  #22672 ) ;
#19284 = DIRECTION ( 'NONE',  ( 7.125109674364536131E-05, -0.9999848031710253382, 0.005512562950849705760 ) ) ;
#19285 = ORIENTED_EDGE ( 'NONE', *, *, #8353, .F. ) ;
#19286 = CARTESIAN_POINT ( 'NONE',  ( 51.08127105622416053, 111.8896246953612206, -48.10680864709630100 ) ) ;
#19287 = VERTEX_POINT ( 'NONE', #16660 ) ;
#19288 = CARTESIAN_POINT ( 'NONE',  ( -91.62437796271721879, 34.61572286322119396, -60.86849236629028326 ) ) ;
#19289 = FACE_OUTER_BOUND ( 'NONE', #5131, .T. ) ;
#19290 = CARTESIAN_POINT ( 'NONE',  ( -47.06729551376847809, 166.8517785085912237, 277.2517607094216032 ) ) ;
#19291 = ORIENTED_EDGE ( 'NONE', *, *, #11348, .F. ) ;
#19292 = CARTESIAN_POINT ( 'NONE',  ( -5.563703806607757762, 326.7005119474488311, 320.3383740725303710 ) ) ;
#19293 = FILL_AREA_STYLE ('',( #3208 ) ) ;
#19294 = ADVANCED_FACE ( 'NONE', ( #1134 ), #19235, .F. ) ;
#19295 = ORIENTED_EDGE ( 'NONE', *, *, #16350, .F. ) ;
#19296 = CARTESIAN_POINT ( 'NONE',  ( -3.170773005268938238, 326.9713452165928516, 319.6393817883191559 ) ) ;
#19297 = LINE ( 'NONE', #11944, #17784 ) ;
#19298 = EDGE_CURVE ( 'NONE', #8602, #2955, #479, .T. ) ;
#19299 = ORIENTED_EDGE ( 'NONE', *, *, #5185, .F. ) ;
#19300 = CARTESIAN_POINT ( 'NONE',  ( -8.849534454763640312, 81.98100004360546222, -94.75705998267450525 ) ) ;
#19301 = CARTESIAN_POINT ( 'NONE',  ( -90.09224011917365260, 87.50613751784533179, 51.09010363202818894 ) ) ;
#19302 = PRODUCT ( 'Angle Locking Side Clamp', 'Angle Locking Side Clamp', '', ( #7472 ) ) ;
#19304 = ORIENTED_EDGE ( 'NONE', *, *, #17355, .F. ) ;
#19303 = ORIENTED_EDGE ( 'NONE', *, *, #20353, .T. ) ;
#19305 = EDGE_CURVE ( 'NONE', #13285, #16331, #3403, .T. ) ;
#19306 = ORIENTED_EDGE ( 'NONE', *, *, #19044, .T. ) ;
#19307 = DIRECTION ( 'NONE',  ( 0.01035335185279151644, 0.005513005182360133580, 0.9999312050732649393 ) ) ;
#19308 = ADVANCED_FACE ( 'NONE', ( #11815 ), #11931, .F. ) ;
#19309 = ADVANCED_FACE ( 'NONE', ( #12143 ), #12027, .F. ) ;
#19310 = CARTESIAN_POINT ( 'NONE',  ( -35.60051853910361075, 93.98889162522327467, 83.40423953877066765 ) ) ;
#19311 = CARTESIAN_POINT ( 'NONE',  ( 81.24851531246423519, 75.12795917139311541, -5.979890628633788729 ) ) ;
#19312 = DIRECTION ( 'NONE',  ( 0.000000000000000000, 0.000000000000000000, -1.000000000000000000 ) ) ;
#19313 = ORIENTED_EDGE ( 'NONE', *, *, #21029, .T. ) ;
#19314 = EDGE_CURVE ( 'NONE', #7137, #9319, #1218, .T. ) ;
#19315 = CARTESIAN_POINT ( 'NONE',  ( 19.63554660563192300, 184.7628467462468791, 276.5100505641262316 ) ) ;
#19316 = ORIENTED_EDGE ( 'NONE', *, *, #4125, .T. ) ;
#19317 = CARTESIAN_POINT ( 'NONE',  ( -35.42010074854528767, 108.0982075334647163, 199.8475074598744357 ) ) ;
#19318 = CARTESIAN_POINT ( 'NONE',  ( -77.67539104474651879, 75.11021523748624418, 5.579831338258102846 ) ) ;
#19319 = CARTESIAN_POINT ( 'NONE',  ( -24.90374348704198226, 324.4871656374173199, 319.9339819361791228 ) ) ;
#19320 = CARTESIAN_POINT ( 'NONE',  ( 88.41758806590424058, 80.31838830481383695, -32.48564084813595798 ) ) ;
#19321 = CYLINDRICAL_SURFACE ( 'NONE', #2299, 7.499999999999992006 ) ;
#19322 = DIRECTION ( 'NONE',  ( -0.01292394549866745720, -0.005513023399720816918, -0.9999012842304692006 ) ) ;
#19323 = CARTESIAN_POINT ( 'NONE',  ( 48.42481440403541626, 171.1166637882075463, 267.9931995069536583 ) ) ;
#19324 = ADVANCED_FACE ( 'NONE', ( #13763 ), #1578, .T. ) ;
#19325 = ORIENTED_EDGE ( 'NONE', *, *, #3026, .F. ) ;
#19326 = EDGE_CURVE ( 'NONE', #14680, #20163, #16994, .T. ) ;
#19327 = DIRECTION ( 'NONE',  ( 0.01246513159389315249, 0.2641402835564749529, 0.9644037178988122960 ) ) ;
#19328 = VERTEX_POINT ( 'NONE', #5576 ) ;
#19329 = EDGE_LOOP ( 'NONE', ( #12574, #17584 ) ) ;
#19330 = ORIENTED_EDGE ( 'NONE', *, *, #15841, .F. ) ;
#19331 = EDGE_CURVE ( 'NONE', #12084, #18197, #12721, .T. ) ;
#19332 = DIRECTION ( 'NONE',  ( -7.125109674160258889E-05, 0.9999848031710252272, -0.005512562950849897447 ) ) ;
#19334 = EDGE_LOOP ( 'NONE', ( #248, #4113, #12194 ) ) ;
#19333 = EDGE_LOOP ( 'NONE', ( #6507, #18574, #3873, #2063, #9839 ) ) ;
#19335 = AXIS2_PLACEMENT_3D ( 'NONE', #8628, #11989, #12102 ) ;
#19336 = ADVANCED_FACE ( 'NONE', ( #12608 ), #422, .F. ) ;
#19337 = DIRECTION ( 'NONE',  ( -1.000000000000000000, 0.000000000000000000, -1.372099599554306628E-14 ) ) ;
#19338 = DIRECTION ( 'NONE',  ( -0.000000000000000000, -1.000000000000000000, -0.000000000000000000 ) ) ;
#19339 = FACE_OUTER_BOUND ( 'NONE', #1787, .T. ) ;
#19340 = CARTESIAN_POINT ( 'NONE',  ( -2.067862704742604141, 69.99999999999998579, -159.9866367664322979 ) ) ;
#19341 = CARTESIAN_POINT ( 'NONE',  ( -55.40268456415265774, 20.00000000000000000, -113.1659955246495741 ) ) ;
#19342 = ADVANCED_FACE ( 'NONE', ( #17790 ), #12380, .T. ) ;
#19343 = PRESENTATION_STYLE_ASSIGNMENT (( #1778 ) ) ;
#19344 = CARTESIAN_POINT ( 'NONE',  ( 81.92940647337731264, 75.18465056264352597, -6.980012735552315384 ) ) ;
#19345 = CARTESIAN_POINT ( 'NONE',  ( 18.36248364585371817, 184.0714940213935904, 310.1538024246328860 ) ) ;
#19346 = CARTESIAN_POINT ( 'NONE',  ( 90.50635355031315044, 79.35163122866354968, 27.25632624755930067 ) ) ;
#19347 = LINE ( 'NONE', #16283, #10655 ) ;
#19348 = EDGE_LOOP ( 'NONE', ( #9790, #5558, #6091, #19995 ) ) ;
#19349 = AXIS2_PLACEMENT_3D ( 'NONE', #11388, #950, #21921 ) ;
#19350 = EDGE_CURVE ( 'NONE', #18453, #21547, #6622, .T. ) ;
#19351 = LINE ( 'NONE', #3849, #6259 ) ;
#19352 = DIRECTION ( 'NONE',  ( -0.01292414190464131335, -1.902755938799530239E-22, -0.9999164797902015955 ) ) ;
#19353 = ORIENTED_EDGE ( 'NONE', *, *, #2325, .T. ) ;
#19354 = CARTESIAN_POINT ( 'NONE',  ( -89.33542534687488512, 79.97945796766208559, -29.20190675877561759 ) ) ;
#19355 = ORIENTED_EDGE ( 'NONE', *, *, #17103, .F. ) ;
#19356 = CARTESIAN_POINT ( 'NONE',  ( -14.53254043310009358, 177.6255169206013989, 113.6379760112694584 ) ) ;
#19357 = CARTESIAN_POINT ( 'NONE',  ( -10.91468522650879258, 105.6685712077031241, 121.5997949944007246 ) ) ;
#19358 = DIRECTION ( 'NONE',  ( -0.1337561903331546953, -0.9909881666746205298, 0.007192708699472573526 ) ) ;
#19359 = MECHANICAL_DESIGN_GEOMETRIC_PRESENTATION_REPRESENTATION (  '', ( #21196 ), #9460 ) ;
#19360 = DIRECTION ( 'NONE',  ( 0.01292394549866738608, 0.005513023399720699824, 0.9999012842304692006 ) ) ;
#19361 = EDGE_CURVE ( 'NONE', #559, #8785, #5226, .T. ) ;
#19362 = ORIENTED_EDGE ( 'NONE', *, *, #6704, .F. ) ;
#19363 = CARTESIAN_POINT ( 'NONE',  ( 13.09069504930537597, 190.2760544069976163, 320.8462072796203302 ) ) ;
#19364 = CARTESIAN_POINT ( 'NONE',  ( 10.29247160983360843, 159.4782971220276693, 81.53177573179129922 ) ) ;
#19365 = CARTESIAN_POINT ( 'NONE',  ( -66.06691928577359363, 94.02752048664900997, -82.12548041065298321 ) ) ;
#19366 = CARTESIAN_POINT ( 'NONE',  ( 51.58262974252190958, 107.1441749712451639, 69.90890102575978915 ) ) ;
#19368 = CARTESIAN_POINT ( 'NONE',  ( -2.000285031460988794, 141.9874903446699363, 256.8043760453134610 ) ) ;
#19367 = CARTESIAN_POINT ( 'NONE',  ( -10.89406810251570867, 163.6808686305110143, 123.6704018889790717 ) ) ;
#19369 = LINE ( 'NONE', #3635, #9195 ) ;
#19370 = VERTEX_POINT ( 'NONE', #8782 ) ;
#19371 = VECTOR ( 'NONE', #1461, 999.9999999999998863 ) ;
#19372 = CARTESIAN_POINT ( 'NONE',  ( -11.21443378733192020, 186.6088958083097680, 308.4147112809631039 ) ) ;
#19373 = VERTEX_POINT ( 'NONE', #12266 ) ;
#19374 = CARTESIAN_POINT ( 'NONE',  ( -40.92987198850381958, 97.39926864640101201, 83.83894969480016357 ) ) ;
#19375 = CARTESIAN_POINT ( 'NONE',  ( 15.77462424665207763, 168.0465177001844665, 307.9256531486020094 ) ) ;
#19376 = CARTESIAN_POINT ( 'NONE',  ( -15.03921139472108415, 178.6409456330145531, 315.6521442976429057 ) ) ;
#19377 = ORIENTED_EDGE ( 'NONE', *, *, #10333, .T. ) ;
#19378 = VECTOR ( 'NONE', #10608, 1000.000000000000000 ) ;
#19379 = CYLINDRICAL_SURFACE ( 'NONE', #7687, 6.499999999999998224 ) ;
#19380 = FACE_OUTER_BOUND ( 'NONE', #11176, .T. ) ;
#19381 = CARTESIAN_POINT ( 'NONE',  ( -10.91052170081621853, 113.6767190643319196, 123.0557169659435459 ) ) ;
#19382 = FACE_OUTER_BOUND ( 'NONE', #17377, .T. ) ;
#19383 = DIRECTION ( 'NONE',  ( 2.025474946048326158E-22, -1.000000000000000000, 1.876735158486678933E-22 ) ) ;
#19384 = AXIS2_PLACEMENT_3D ( 'NONE', #2468, #18116, #7968 ) ;
#19385 = ORIENTED_EDGE ( 'NONE', *, *, #19495, .F. ) ;
#19386 = DIRECTION ( 'NONE',  ( -0.1296504907605108559, -0.005475273188901296634, -0.9915446392518419971 ) ) ;
#19387 = DIRECTION ( 'NONE',  ( 0.01292394549867042185, 0.005513023399718316314, 0.9999012842304693116 ) ) ;
#19388 = EDGE_CURVE ( 'NONE', #1243, #21215, #19687, .T. ) ;
#19389 = FACE_OUTER_BOUND ( 'NONE', #8064, .T. ) ;
#19390 = EDGE_CURVE ( 'NONE', #12054, #11089, #7072, .T. ) ;
#19391 = AXIS2_PLACEMENT_3D ( 'NONE', #20906, #1846, #4939 ) ;
#19392 = CARTESIAN_POINT ( 'NONE',  ( 49.56017638316297536, 109.8092428479078961, -47.32487478585164808 ) ) ;
#19393 = ORIENTED_EDGE ( 'NONE', *, *, #22105, .F. ) ;
#19394 = EDGE_LOOP ( 'NONE', ( #8497, #19165, #19598, #18139 ) ) ;
#19395 = CARTESIAN_POINT ( 'NONE',  ( -48.91844876508264406, 94.45452722259994971, 84.00069590936301722 ) ) ;
#19396 = DIRECTION ( 'NONE',  ( -0.01292414190464131335, -1.902755938799530239E-22, -0.9999164797902015955 ) ) ;
#19397 = ORIENTED_EDGE ( 'NONE', *, *, #10367, .T. ) ;
#19398 = CARTESIAN_POINT ( 'NONE',  ( 51.42485355984464945, 109.2346207959984241, -44.83403687369097668 ) ) ;
#19399 = ORIENTED_EDGE ( 'NONE', *, *, #22511, .F. ) ;
#19400 = SHAPE_REPRESENTATION_RELATIONSHIP ( 'NONE' , 'NONE' ,  #19567, #2240 ) ;
#19401 = DIRECTION ( 'NONE',  ( -0.1136178953597573593, 0.9935164314186355483, -0.004009283626633517415 ) ) ;
#19402 = DIRECTION ( 'NONE',  ( 0.1296504907605108559, 0.005475273188901296634, 0.9915446392518419971 ) ) ;
#19403 = DIRECTION ( 'NONE',  ( 0.9999164797902015955, 6.965998958219364448E-18, -0.01292414190464157182 ) ) ;
#19404 = DIRECTION ( 'NONE',  ( 7.125109674160325297E-05, -0.9999848031710252272, 0.005512562950849327591 ) ) ;
#19405 = DIRECTION ( 'NONE',  ( 0.9999164797902015955, 0.000000000000000000, -0.01292414190463754553 ) ) ;
#19406 = CARTESIAN_POINT ( 'NONE',  ( -51.82774057240565213, 118.9447701193097942, 172.1955447453271404 ) ) ;
#19407 = AXIS2_PLACEMENT_3D ( 'NONE', #6644, #13671, #15738 ) ;
#19408 = ORIENTED_EDGE ( 'NONE', *, *, #6195, .F. ) ;
#19409 = DIRECTION ( 'NONE',  ( -0.006837993415046672921, -0.8485676841065771248, -0.5290426517172845955 ) ) ;
#19410 = CARTESIAN_POINT ( 'NONE',  ( -89.59931147023513631, 89.08017288857402605, 51.79292875781501948 ) ) ;
#19411 = ORIENTED_EDGE ( 'NONE', *, *, #19298, .T. ) ;
#19412 = EDGE_CURVE ( 'NONE', #3703, #7715, #18008, .T. ) ;
#19413 = ORIENTED_EDGE ( 'NONE', *, *, #7053, .T. ) ;
#19414 = FACE_OUTER_BOUND ( 'NONE', #17513, .T. ) ;
#19415 = CARTESIAN_POINT ( 'NONE',  ( -10.85624112972181621, 113.6998737626107641, 127.2553023597115214 ) ) ;
#19416 = AXIS2_PLACEMENT_3D ( 'NONE', #6600, #16973, #5295 ) ;
#19417 = EDGE_CURVE ( 'NONE', #726, #22603, #8547, .T. ) ;
#19418 = FACE_OUTER_BOUND ( 'NONE', #12793, .T. ) ;
#19419 = CARTESIAN_POINT ( 'NONE',  ( 83.15649767528586267, 75.08639547911840850, 2.980377557322682502 ) ) ;
#19420 = AXIS2_PLACEMENT_3D ( 'NONE', #6684, #17052, #20694 ) ;
#19421 = FACE_OUTER_BOUND ( 'NONE', #14517, .T. ) ;
#19422 = ORIENTED_EDGE ( 'NONE', *, *, #710, .F. ) ;
#19423 = DIRECTION ( 'NONE',  ( 0.000000000000000000, 0.000000000000000000, 1.000000000000000000 ) ) ;
#19424 = ORIENTED_EDGE ( 'NONE', *, *, #4969, .T. ) ;
#19425 = CARTESIAN_POINT ( 'NONE',  ( -55.17377582547666037, 114.2470151460891827, 172.6590000314777456 ) ) ;
#19426 = AXIS2_PLACEMENT_3D ( 'NONE', #2147, #17688, #10777 ) ;
#19427 = CARTESIAN_POINT ( 'NONE',  ( -10.85795115604361349, 137.6995090387153482, 127.1230008488911096 ) ) ;
#19428 = CARTESIAN_POINT ( 'NONE',  ( -77.38242492463166400, 75.10273324658501792, 5.418133580374851377 ) ) ;
#19429 = CARTESIAN_POINT ( 'NONE',  ( -25.69698422022063866, 324.3509299035710001, 308.6536381847947155 ) ) ;
#19430 = ORIENTED_EDGE ( 'NONE', *, *, #9930, .T. ) ;
#19431 = CARTESIAN_POINT ( 'NONE',  ( -105.4610200154982920, 77.75225708752505227, 31.27258767819528984 ) ) ;
#19432 = ORIENTED_EDGE ( 'NONE', *, *, #16832, .F. ) ;
#19433 = LINE ( 'NONE', #14065, #22079 ) ;
#19434 = PRESENTATION_STYLE_ASSIGNMENT (( #22515 ) ) ;
#19435 = CARTESIAN_POINT ( 'NONE',  ( 3.600049111542418689, 166.5356125545590373, 278.5290088303507332 ) ) ;
#19436 = VERTEX_POINT ( 'NONE', #7192 ) ;
#19437 = ADVANCED_FACE ( 'NONE', ( #2250 ), #17897, .F. ) ;
#19438 = CARTESIAN_POINT ( 'NONE',  ( -154.0000000000000000, 20.00000000000000000, -53.76161406891256433 ) ) ;
#19439 = VERTEX_POINT ( 'NONE', #3861 ) ;
#19440 = CIRCLE ( 'NONE', #2931, 11.00000000000000178 ) ;
#19441 = ORIENTED_EDGE ( 'NONE', *, *, #13113, .T. ) ;
#19442 = VECTOR ( 'NONE', #6478, 1000.000000000000000 ) ;
#19443 = DIRECTION ( 'NONE',  ( 0.01292414190463830014, 0.000000000000000000, 0.9999164797902017066 ) ) ;
#19444 = PRODUCT_DEFINITION_FORMATION_WITH_SPECIFIED_SOURCE ( 'ANY', '', #20165, .NOT_KNOWN. ) ;
#19446 = ORIENTED_EDGE ( 'NONE', *, *, #20307, .T. ) ;
#19445 = VERTEX_POINT ( 'NONE', #14460 ) ;
#19447 = CARTESIAN_POINT ( 'NONE',  ( 40.87255160414490973, 95.04007462656775829, -44.54585608918304729 ) ) ;
#19448 = FACE_OUTER_BOUND ( 'NONE', #224, .T. ) ;
#19449 = ADVANCED_FACE ( 'NONE', ( #3956 ), #1236, .F. ) ;
#19450 = CARTESIAN_POINT ( 'NONE',  ( 3.833582208902202471, 166.6352317792378415, 296.5970240496424708 ) ) ;
#19451 = CARTESIAN_POINT ( 'NONE',  ( -40.80932907711049751, 95.23503300788487991, 83.16719596654198199 ) ) ;
#19452 = EDGE_CURVE ( 'NONE', #20449, #15161, #5451, .T. ) ;
#19453 = CARTESIAN_POINT ( 'NONE',  ( 13.01890817498768449, 190.3110758050131892, 320.8522954438618058 ) ) ;
#19454 = CARTESIAN_POINT ( 'NONE',  ( 76.79553162410384459, 75.15439084847217543, -6.407829649116825621 ) ) ;
#19455 = CARTESIAN_POINT ( 'NONE',  ( 13.46034337553667193, 187.1166012126664668, 307.7207322155608153 ) ) ;
#19456 = CARTESIAN_POINT ( 'NONE',  ( 91.78322154246586706, 80.00947954930573758, 29.27761720249711530 ) ) ;
#19457 = VECTOR ( 'NONE', #3179, 1000.000000000000000 ) ;
#19458 = DIRECTION ( 'NONE',  ( 7.125109674161246868E-05, -0.9999848031710253382, 0.005512562950850155054 ) ) ;
#19459 = TOROIDAL_SURFACE ( 'NONE', #9187, 85.00000000000000000, 2.000000000000000000 ) ;
#19460 = ADVANCED_FACE ( 'NONE', ( #5686 ), #17669, .F. ) ;
#19461 = DIRECTION ( 'NONE',  ( -0.009138748381789079875, -0.7071067811865487940, -0.7070477234798316912 ) ) ;
#19462 = CIRCLE ( 'NONE', #22375, 3.047499999999988329 ) ;
#19463 = DIRECTION ( 'NONE',  ( -0.01292394549866740169, -0.005513023399721131770, -0.9999012842304693116 ) ) ;
#19464 = ORIENTED_EDGE ( 'NONE', *, *, #20826, .F. ) ;
#19465 = CARTESIAN_POINT ( 'NONE',  ( -91.69446324238904822, 77.56197482480477845, -29.51646066538620161 ) ) ;
#19466 = EDGE_LOOP ( 'NONE', ( #20320, #17406, #13366, #5535 ) ) ;
#19467 = EDGE_CURVE ( 'NONE', #4369, #17908, #15192, .T. ) ;
#19468 = CIRCLE ( 'NONE', #11061, 9.000000000000001776 ) ;
#19469 = CARTESIAN_POINT ( 'NONE',  ( -63.91682626075579066, 94.48610424851698042, 84.22316112083727546 ) ) ;
#19470 = DIRECTION ( 'NONE',  ( 0.01035335185279153900, 0.005513005182355262476, 0.9999312050732647172 ) ) ;
#19471 = AXIS2_PLACEMENT_3D ( 'NONE', #21484, #4482, #11169 ) ;
#19472 = DIRECTION ( 'NONE',  ( 0.01105745575040835080, 0.5176938329688192120, 0.8554944932484254139 ) ) ;
#19473 = DIRECTION ( 'NONE',  ( 0.01292394549866738782, 0.005513023399720468239, 0.9999012842304692006 ) ) ;
#19474 = ADVANCED_FACE ( 'NONE', ( #13074, #2820 ), #18228, .T. ) ;
#19475 = CIRCLE ( 'NONE', #20939, 126.0000000000000000 ) ;
#19476 = ORIENTED_EDGE ( 'NONE', *, *, #11768, .F. ) ;
#19477 = CARTESIAN_POINT ( 'NONE',  ( -17.78132405376864966, 81.99999999999998579, -83.07604999942009272 ) ) ;
#19478 = VERTEX_POINT ( 'NONE', #6042 ) ;
#19479 = LINE ( 'NONE', #3751, #2733 ) ;
#19480 = DIRECTION ( 'NONE',  ( -0.9934404589540162256, -0.1135548637187057258, 0.01346653032743021748 ) ) ;
#19481 = CARTESIAN_POINT ( 'NONE',  ( -11.40735840365825915, 183.0524750669056004, 320.8439791889416028 ) ) ;
#19482 = ADVANCED_BREP_SHAPE_REPRESENTATION ( '', ( #9632, #6292 ), #7747 ) ;
#19483 = CARTESIAN_POINT ( 'NONE',  ( -91.40888322292894941, 77.29711350638248746, 31.45985873596569959 ) ) ;
#19484 = DIRECTION ( 'NONE',  ( 0.006717398120142096217, -0.8543148575185137705, 0.5197124212346833083 ) ) ;
#19485 = ORIENTED_EDGE ( 'NONE', *, *, #7864, .T. ) ;
#19486 = CARTESIAN_POINT ( 'NONE',  ( -14.04492576652437918, 182.2513542422996693, 310.6408630182388038 ) ) ;
#19487 = CIRCLE ( 'NONE', #15491, 1.999999999999998446 ) ;
#19488 = PRODUCT_DEFINITION_SHAPE ( 'NONE', 'NONE',  #12273 ) ;
#19489 = FACE_OUTER_BOUND ( 'NONE', #5865, .T. ) ;
#19490 = CARTESIAN_POINT ( 'NONE',  ( 17.98832021580386353, 168.3016772219343693, 308.4219264720497904 ) ) ;
#19491 = CARTESIAN_POINT ( 'NONE',  ( -15.09479064048255381, 179.6969842254679861, 315.8799336093683792 ) ) ;
#19492 = AXIS2_PLACEMENT_3D ( 'NONE', #4945, #6790, #5054 ) ;
#19493 = ADVANCED_FACE ( 'NONE', ( #20039, #4297 ), #13177, .T. ) ;
#19494 = FACE_OUTER_BOUND ( 'NONE', #17169, .T. ) ;
#19495 = EDGE_CURVE ( 'NONE', #8011, #8602, #17755, .T. ) ;
#19496 = VECTOR ( 'NONE', #7511, 1000.000000000000114 ) ;
#19497 = ORIENTED_EDGE ( 'NONE', *, *, #11629, .F. ) ;
#19498 = DIRECTION ( 'NONE',  ( 0.9232306267972774094, 0.000000000000000000, -0.3842462878721227826 ) ) ;
#19499 = CONTEXT_DEPENDENT_SHAPE_REPRESENTATION ( #617, #1874 ) ;
#19500 = CARTESIAN_POINT ( 'NONE',  ( 37.86419661074339871, 93.64690829566114871, 82.87065082833630925 ) ) ;
#19501 = VECTOR ( 'NONE', #20783, 1000.000000000000114 ) ;
#19502 = AXIS2_PLACEMENT_3D ( 'NONE', #459, #9165, #12648 ) ;
#19503 = DIRECTION ( 'NONE',  ( -0.000000000000000000, -1.000000000000000000, -0.000000000000000000 ) ) ;
#19504 = EDGE_CURVE ( 'NONE', #5306, #10057, #2718, .T. ) ;
#19505 = CARTESIAN_POINT ( 'NONE',  ( -3.719543892204659752, 174.4361193905359642, 323.6543047440632108 ) ) ;
#19506 = LINE ( 'NONE', #8817, #1227 ) ;
#19507 = EDGE_LOOP ( 'NONE', ( #10866, #17488, #865, #2082 ) ) ;
#19508 = AXIS2_PLACEMENT_3D ( 'NONE', #12887, #16574, #5977 ) ;
#19509 = VERTEX_POINT ( 'NONE', #21969 ) ;
#19510 = CARTESIAN_POINT ( 'NONE',  ( 38.46180957136368761, 93.08398165842311300, -84.42015501544466360 ) ) ;
#19511 = CARTESIAN_POINT ( 'NONE',  ( 14.19424140980583537, 137.7226637369942068, 130.9994826950430422 ) ) ;
#19512 = ORIENTED_EDGE ( 'NONE', *, *, #10480, .T. ) ;
#19513 = CARTESIAN_POINT ( 'NONE',  ( -49.63640462543862242, 95.17726600392212788, -43.75321583467091813 ) ) ;
#19514 = AXIS2_PLACEMENT_3D ( 'NONE', #9802, #4500, #8061 ) ;
#19515 = ORIENTED_EDGE ( 'NONE', *, *, #21659, .F. ) ;
#19516 = FACE_OUTER_BOUND ( 'NONE', #4935, .T. ) ;
#19517 = CYLINDRICAL_SURFACE ( 'NONE', #20693, 2.000000000000001776 ) ;
#19518 = CARTESIAN_POINT ( 'NONE',  ( 4.376210989365964643, 81.99999999999998579, -92.29796090835097289 ) ) ;
#19519 = DIRECTION ( 'NONE',  ( -0.9999164797902015955, -2.001050586450181282E-22, 0.01292414190463992731 ) ) ;
#19520 = APPLICATION_CONTEXT ( 'automotive_design' ) ;
#19521 = CARTESIAN_POINT ( 'NONE',  ( 37.04297230413862962, 93.86474644718838078, 82.35129237346917819 ) ) ;
#19522 = B_SPLINE_CURVE_WITH_KNOTS ( 'NONE', 3,
 ( #22510, #20585, #20364, #2908, #1650, #9919, #17272, #16944 ),
 .UNSPECIFIED., .F., .F.,
 ( 4, 2, 2, 4 ),
 ( 6.938893903907228378E-18, 0.0005562605569428313076, 0.001112521113885655676, 0.002225042227771339108 ),
 .UNSPECIFIED. ) ;
#19523 = VECTOR ( 'NONE', #17119, 999.9999999999998863 ) ;
#19524 = AXIS2_PLACEMENT_3D ( 'NONE', #4913, #6437, #6757 ) ;
#19525 = AXIS2_PLACEMENT_3D ( 'NONE', #12823, #7539, #16820 ) ;
#19526 = CARTESIAN_POINT ( 'NONE',  ( 16.60733960726993530, 168.1940330716068388, 320.8824762435588127 ) ) ;
#19527 = EDGE_CURVE ( 'NONE', #6141, #6699, #18562, .T. ) ;
#19528 = EDGE_CURVE ( 'NONE', #440, #4475, #19190, .T. ) ;
#19529 = ORIENTED_EDGE ( 'NONE', *, *, #14846, .T. ) ;
#19530 = LINE ( 'NONE', #353, #5820 ) ;
#19531 = CARTESIAN_POINT ( 'NONE',  ( -90.08557003309165623, 87.52532468786372988, 51.07836697400083636 ) ) ;
#19532 = AXIS2_PLACEMENT_3D ( 'NONE', #15747, #8696, #6654 ) ;
#19533 = ADVANCED_BREP_SHAPE_REPRESENTATION ( '', ( #17376, #6292 ), #8126 ) ;
#19534 = CIRCLE ( 'NONE', #17167, 2.000000000000004441 ) ;
#19535 = ORIENTED_EDGE ( 'NONE', *, *, #3070, .T. ) ;
#19536 = ORIENTED_EDGE ( 'NONE', *, *, #1683, .T. ) ;
#19537 = CARTESIAN_POINT ( 'NONE',  ( -106.2089377515398780, 72.00000000000000000, -28.62973177816246206 ) ) ;
#19538 = DIRECTION ( 'NONE',  ( 0.000000000000000000, 0.000000000000000000, 1.000000000000000000 ) ) ;
#19539 = AXIS2_PLACEMENT_3D ( 'NONE', #2740, #6176, #9751 ) ;
#19540 = CARTESIAN_POINT ( 'NONE',  ( -105.7941983518662852, 70.06152065884128888, -30.12648231254621933 ) ) ;
#19541 = AXIS2_PLACEMENT_3D ( 'NONE', #9431, #842, #7940 ) ;
#19542 = DIRECTION ( 'NONE',  ( -0.01292394549866744159, -0.005513023399721241925, -0.9999012842304693116 ) ) ;
#19543 = ORIENTED_EDGE ( 'NONE', *, *, #21263, .F. ) ;
#19544 = CARTESIAN_POINT ( 'NONE',  ( 48.56361546678319030, 189.3893605493459233, -111.4534788612804732 ) ) ;
#19545 = ORIENTED_EDGE ( 'NONE', *, *, #8003, .T. ) ;
#19546 = CARTESIAN_POINT ( 'NONE',  ( -1.124400345703740589, 72.00000000000000000, -86.99273374174759965 ) ) ;
#19547 = CARTESIAN_POINT ( 'NONE',  ( -38.21549050681395698, 167.4026153394593734, 273.1339171915171846 ) ) ;
#19548 = CARTESIAN_POINT ( 'NONE',  ( -75.03994275328706465, 75.00864948959272738, 2.293017013057943032 ) ) ;
#19549 = CARTESIAN_POINT ( 'NONE',  ( -10.33200872664665049, 165.0651399145666005, 308.9564794664337342 ) ) ;
#19550 = VERTEX_POINT ( 'NONE', #6270 ) ;
#19551 = DIRECTION ( 'NONE',  ( -7.125109674161259066E-05, 0.9999848031710252272, -0.005512562950850163727 ) ) ;
#19552 = VERTEX_POINT ( 'NONE', #11325 ) ;
#19553 = CARTESIAN_POINT ( 'NONE',  ( -38.21549050681395698, 167.4026153394593734, 273.1339171915171846 ) ) ;
#19554 = CARTESIAN_POINT ( 'NONE',  ( 65.34146690339817098, 126.1473081376433498, 25.99859803869739139 ) ) ;
#19555 = ORIENTED_EDGE ( 'NONE', *, *, #1116, .F. ) ;
#19556 = EDGE_CURVE ( 'NONE', #21410, #5718, #7823, .T. ) ;
#19557 = CARTESIAN_POINT ( 'NONE',  ( -1.163172771417702700, 70.69320546282760631, -89.99248318111824574 ) ) ;
#19558 = ORIENTED_EDGE ( 'NONE', *, *, #5020, .F. ) ;
#19559 = VECTOR ( 'NONE', #5342, 1000.000000000000000 ) ;
#19560 = ORIENTED_EDGE ( 'NONE', *, *, #17750, .T. ) ;
#19561 = CARTESIAN_POINT ( 'NONE',  ( -15.05589034484066246, 113.6998737626107641, 127.3095837557110315 ) ) ;
#19562 = ORIENTED_EDGE ( 'NONE', *, *, #16379, .F. ) ;
#19563 = DIRECTION ( 'NONE',  ( 0.01111468050521610164, -0.5103046645782707280, 0.8599218645824314722 ) ) ;
#19564 = CARTESIAN_POINT ( 'NONE',  ( 58.87479767622038906, 143.5880916635284166, 105.9939182712553105 ) ) ;
#19565 = CARTESIAN_POINT ( 'NONE',  ( -1.079165849037536207, 45.00000000000000000, -83.49302606248184588 ) ) ;
#19566 = DIRECTION ( 'NONE',  ( 0.3101392564284308762, 0.9506461370142480494, -0.009250070373106863975 ) ) ;
#19567 = SHAPE_REPRESENTATION ( 'Hex Screw', ( #6292 ), #20203 ) ;
#19568 = CARTESIAN_POINT ( 'NONE',  ( 75.80607982450202087, 75.11648168028638395, -5.692233723461522565 ) ) ;
#19569 = CARTESIAN_POINT ( 'NONE',  ( 19.13497996244607080, 183.4159916094967571, 311.1842790287917069 ) ) ;
#19570 = AXIS2_PLACEMENT_3D ( 'NONE', #9545, #20090, #11271 ) ;
#19571 = CARTESIAN_POINT ( 'NONE',  ( 89.40485731804140812, 79.89806915697582212, 28.95844815008357287 ) ) ;
#19572 = AXIS2_PLACEMENT_3D ( 'NONE', #4049, #19665, #21727 ) ;
#19573 = FACE_OUTER_BOUND ( 'NONE', #1862, .T. ) ;
#19574 = ORIENTED_EDGE ( 'NONE', *, *, #12924, .F. ) ;
#19575 = CARTESIAN_POINT ( 'NONE',  ( -14.16912629561661063, 163.6990670166405266, 127.0139394094123304 ) ) ;
#19576 = EDGE_LOOP ( 'NONE', ( #12987, #15028, #21533, #11848 ) ) ;
#19577 = AXIS2_PLACEMENT_3D ( 'NONE', #6099, #13125, #20095 ) ;
#19578 = CARTESIAN_POINT ( 'NONE',  ( 45.44350069997184249, 168.6907664596096765, 34.02200722522287180 ) ) ;
#19579 = ADVANCED_FACE ( 'NONE', ( #20270 ), #18819, .F. ) ;
#19580 = ORIENTED_EDGE ( 'NONE', *, *, #1103, .T. ) ;
#19581 = AXIS2_PLACEMENT_3D ( 'NONE', #18133, #11110, #5797 ) ;
#19582 = VECTOR ( 'NONE', #17797, 1000.000000000000114 ) ;
#19583 = ORIENTED_EDGE ( 'NONE', *, *, #17815, .T. ) ;
#19584 = CARTESIAN_POINT ( 'NONE',  ( -5.156377330703347361, 70.80384757729338219, -99.58697729741749072 ) ) ;
#19585 = SURFACE_STYLE_USAGE ( .BOTH. , #12604 ) ;
#19586 = CARTESIAN_POINT ( 'NONE',  ( -88.18357460598782893, 87.01269140057722495, 51.36456657205789611 ) ) ;
#19587 = EDGE_CURVE ( 'NONE', #6191, #7136, #7636, .T. ) ;
#19588 = EDGE_LOOP ( 'NONE', ( #10811, #17781, #18262 ) ) ;
#19589 = CARTESIAN_POINT ( 'NONE',  ( -41.52238611146465530, 166.0448094368136935, 269.1837510020998820 ) ) ;
#19590 = ORIENTED_EDGE ( 'NONE', *, *, #2650, .F. ) ;
#19591 = CIRCLE ( 'NONE', #3467, 3.047499999999998987 ) ;
#19592 = DIRECTION ( 'NONE',  ( 0.09199399308265900077, -0.9957502728239346901, 0.004301093787334665970 ) ) ;
#19593 = EDGE_CURVE ( 'NONE', #20328, #10931, #8102, .T. ) ;
#19594 = DIRECTION ( 'NONE',  ( -0.9999164797902017066, -6.965998958219367529E-18, 0.01292414190464157182 ) ) ;
#19595 = CARTESIAN_POINT ( 'NONE',  ( -91.85126960211907488, 79.84876637418224732, 31.24149931482875786 ) ) ;
#19596 = DIRECTION ( 'NONE',  ( 0.9999164797902017066, 2.001050586450180576E-22, -0.01292414190464044946 ) ) ;
#19597 = AXIS2_PLACEMENT_3D ( 'NONE', #16409, #11331, #654 ) ;
#19598 = ORIENTED_EDGE ( 'NONE', *, *, #15459, .T. ) ;
#19599 = CARTESIAN_POINT ( 'NONE',  ( -15.03272297201332819, 179.8527073090512545, 316.2340475952451584 ) ) ;
#19600 = ORIENTED_EDGE ( 'NONE', *, *, #11113, .T. ) ;
#19601 = DIRECTION ( 'NONE',  ( 7.125109674403277385E-05, -0.9999848031710253382, 0.005512562950848281552 ) ) ;
#19602 = DIRECTION ( 'NONE',  ( -7.125109674160258889E-05, 0.9999848031710252272, -0.005512562950849897447 ) ) ;
#19603 = CARTESIAN_POINT ( 'NONE',  ( -15.17825613376442284, 179.5172115246878377, 314.3122088330735551 ) ) ;
#19604 = EDGE_CURVE ( 'NONE', #6519, #8189, #12825, .T. ) ;
#19605 = DIRECTION ( 'NONE',  ( -7.125109674364534776E-05, 0.9999848031710252272, -0.005512562950849704026 ) ) ;
#19606 = EDGE_CURVE ( 'NONE', #567, #10181, #17009, .T. ) ;
#19607 = EDGE_CURVE ( 'NONE', #2673, #16738, #18323, .T. ) ;
#19608 = AXIS2_PLACEMENT_3D ( 'NONE', #16028, #6701, #20709 ) ;
#19609 = ADVANCED_FACE ( 'NONE', ( #2378 ), #9369, .T. ) ;
#19610 = CARTESIAN_POINT ( 'NONE',  ( 53.19480552330409751, 129.3639651298425406, 246.8529597961802438 ) ) ;
#19611 = CONTEXT_DEPENDENT_SHAPE_REPRESENTATION ( #15157, #6618 ) ;
#19612 = ORIENTED_EDGE ( 'NONE', *, *, #20483, .T. ) ;
#19613 = FACE_OUTER_BOUND ( 'NONE', #14735, .T. ) ;
#19614 = LINE ( 'NONE', #1717, #16205 ) ;
#19615 = CARTESIAN_POINT ( 'NONE',  ( -13.50073983619024176, 183.7065926015648074, 278.6553669534396249 ) ) ;
#19616 = ORIENTED_EDGE ( 'NONE', *, *, #2935, .F. ) ;
#19617 = DIRECTION ( 'NONE',  ( 0.000000000000000000, 0.000000000000000000, -1.000000000000000000 ) ) ;
#19618 = EDGE_CURVE ( 'NONE', #8537, #19370, #19922, .T. ) ;
#19619 = FACE_OUTER_BOUND ( 'NONE', #5691, .T. ) ;
#19620 = ORIENTED_EDGE ( 'NONE', *, *, #11452, .F. ) ;
#19621 = ORIENTED_EDGE ( 'NONE', *, *, #20150, .F. ) ;
#19622 = DIRECTION ( 'NONE',  ( 0.9999164797902017066, 0.000000000000000000, -0.01292414190463832269 ) ) ;
#19623 = DIRECTION ( 'NONE',  ( 0.000000000000000000, 1.000000000000000000, 0.000000000000000000 ) ) ;
#19624 = VECTOR ( 'NONE', #11147, 1000.000000000000114 ) ;
#19625 = FACE_OUTER_BOUND ( 'NONE', #6221, .T. ) ;
#19626 = CARTESIAN_POINT ( 'NONE',  ( 22.19183229621111053, 88.61243608327089305, 77.38960444610528100 ) ) ;
#19627 = VERTEX_POINT ( 'NONE', #11221 ) ;
#19628 = CARTESIAN_POINT ( 'NONE',  ( 18.98255855869581410, 147.7934693865291536, 278.2536627479764206 ) ) ;
#19629 = FACE_OUTER_BOUND ( 'NONE', #18617, .T. ) ;
#19630 = EDGE_CURVE ( 'NONE', #9213, #15636, #2479, .T. ) ;
#19631 = VERTEX_POINT ( 'NONE', #14918 ) ;
#19632 = CARTESIAN_POINT ( 'NONE',  ( -92.82229925712799457, 69.99999999999998579, 1.199748770783155338 ) ) ;
#19633 = CARTESIAN_POINT ( 'NONE',  ( -88.16803135499490907, 88.64744638044348335, 52.50087471490518709 ) ) ;
#19634 = APPLICATION_PROTOCOL_DEFINITION ( 'draft international standard', 'automotive_design', 1998, #12939 ) ;
#19635 = CIRCLE ( 'NONE', #15284, 124.0000000000000000 ) ;
#19636 = VERTEX_POINT ( 'NONE', #3382 ) ;
#19637 = ORIENTED_EDGE ( 'NONE', *, *, #10688, .F. ) ;
#19638 = CARTESIAN_POINT ( 'NONE',  ( 65.91132412060191825, 106.8061942917681790, 70.08737598725748796 ) ) ;
#19639 = CARTESIAN_POINT ( 'NONE',  ( 1.364374644014609697E-14, 69.99999999999998579, -9.836443712999143722E-15 ) ) ;
#19640 = CARTESIAN_POINT ( 'NONE',  ( -9.065023647928146744, 109.7167603697149474, 130.3064260814875013 ) ) ;
#19641 = CARTESIAN_POINT ( 'NONE',  ( 51.05126519560737108, 95.51270090492249665, 81.01128809578769108 ) ) ;
#19642 = CARTESIAN_POINT ( 'NONE',  ( -33.82085273160089400, 93.50464841319747222, 82.93470554904384073 ) ) ;
#19643 = ORIENTED_EDGE ( 'NONE', *, *, #13488, .T. ) ;
#19644 = ADVANCED_FACE ( 'NONE', ( #3042 ), #20827, .T. ) ;
#19645 = EDGE_LOOP ( 'NONE', ( #7027, #5779, #5699, #10944 ) ) ;
#19646 = DIRECTION ( 'NONE',  ( -0.9999164797902015955, -2.045733645417851681E-15, 0.01292414190464156835 ) ) ;
#19647 = EDGE_CURVE ( 'NONE', #5157, #5306, #22108, .T. ) ;
#19648 = FACE_OUTER_BOUND ( 'NONE', #12922, .T. ) ;
#19649 = PLANE ( 'NONE',  #21528 ) ;
#19650 = CARTESIAN_POINT ( 'NONE',  ( -22.36471611834589623, 324.7801200243509925, 320.5765034992891742 ) ) ;
#19651 = DIRECTION ( 'NONE',  ( -0.01292414190463830014, 0.000000000000000000, -0.9999164797902017066 ) ) ;
#19652 = ORIENTED_EDGE ( 'NONE', *, *, #1841, .F. ) ;
#19653 = DIRECTION ( 'NONE',  ( -0.9999164797902017066, -6.965998958219367529E-18, 0.01292414190464157182 ) ) ;
#19654 = CARTESIAN_POINT ( 'NONE',  ( 4.195452682864886818, 166.7895964344300239, 324.5942600080955458 ) ) ;
#19655 = DIRECTION ( 'NONE',  ( 0.000000000000000000, 0.000000000000000000, 1.000000000000000000 ) ) ;
#19656 = ORIENTED_EDGE ( 'NONE', *, *, #18540, .F. ) ;
#19657 = CARTESIAN_POINT ( 'NONE',  ( -1.247179693797872524, 45.00000000000000000, -96.49194029975447506 ) ) ;
#19658 = ORIENTED_EDGE ( 'NONE', *, *, #219, .F. ) ;
#19659 = ORIENTED_EDGE ( 'NONE', *, *, #21735, .T. ) ;
#19660 = CARTESIAN_POINT ( 'NONE',  ( -84.38495553179255637, 75.03402262061140959, 3.648261192032123734 ) ) ;
#19661 = DIRECTION ( 'NONE',  ( 7.125109674403837105E-05, -0.9999848031710252272, 0.005512562950847867821 ) ) ;
#19662 = ORIENTED_EDGE ( 'NONE', *, *, #20826, .T. ) ;
#19663 = CARTESIAN_POINT ( 'NONE',  ( -3.738111129692070822, 157.0756041464990744, 299.7478936930373266 ) ) ;
#19664 = FACE_BOUND ( 'NONE', #447, .T. ) ;
#19665 = DIRECTION ( 'NONE',  ( 0.01292394549866731149, 0.005513023399720593139, 0.9999012842304692006 ) ) ;
#19666 = EDGE_CURVE ( 'NONE', #17834, #15668, #21382, .T. ) ;
#19667 = EDGE_CURVE ( 'NONE', #6314, #345, #20380, .T. ) ;
#19668 = VECTOR ( 'NONE', #8162, 1000.000000000000000 ) ;
#19669 = FACE_OUTER_BOUND ( 'NONE', #20556, .T. ) ;
#19670 = CARTESIAN_POINT ( 'NONE',  ( 18.51945795647842274, 183.8831096202368087, 308.3970819915673474 ) ) ;
#19671 = CARTESIAN_POINT ( 'NONE',  ( 91.52774025374780820, 80.10656073859405524, 29.55378794065032366 ) ) ;
#19672 =( REPRESENTATION_RELATIONSHIP ('NONE','NONE', #11808, #19567 ) REPRESENTATION_RELATIONSHIP_WITH_TRANSFORMATION ( #20764 )SHAPE_REPRESENTATION_RELATIONSHIP( ) );
#19673 = DIRECTION ( 'NONE',  ( 0.000000000000000000, -1.000000000000000000, 0.000000000000000000 ) ) ;
#19674 = VERTEX_POINT ( 'NONE', #20724 ) ;
#19675 = CARTESIAN_POINT ( 'NONE',  ( -8.375467013762508017, 185.4549566013130857, 322.9624185535398055 ) ) ;
#19676 = CARTESIAN_POINT ( 'NONE',  ( -62.57927418076755544, 119.0295134562299637, 187.7070424667828377 ) ) ;
#19677 = EDGE_LOOP ( 'NONE', ( #889, #4654, #6309, #12350 ) ) ;
#19678 = CARTESIAN_POINT ( 'NONE',  ( -91.78322154246579601, 80.00947954930759920, -29.27761720249670674 ) ) ;
#19679 = ORIENTED_EDGE ( 'NONE', *, *, #6568, .T. ) ;
#19680 = PRODUCT_RELATED_PRODUCT_CATEGORY ( 'part', '', ( #19302 ) ) ;
#19681 = ORIENTED_EDGE ( 'NONE', *, *, #669, .F. ) ;
#19682 = CARTESIAN_POINT ( 'NONE',  ( 63.56236266363622889, 189.3893605493459233, -111.6473409898501075 ) ) ;
#19683 = B_SPLINE_CURVE_WITH_KNOTS ( 'NONE', 3,
 ( #9786, #14522, #14867, #2668, #4256, #6214, #16799, #14753, #18075, #18401 ),
 .UNSPECIFIED., .F., .F.,
 ( 4, 2, 2, 2, 4 ),
 ( -3.258122103471980917E-05, 0.003484391791828234802, 0.007001364804691189922, 0.01051833781755414331, 0.01403531083041709843 ),
 .UNSPECIFIED. ) ;
#19684 = CARTESIAN_POINT ( 'NONE',  ( 14.14224087380716455, 105.6999953372425409, 126.9762993157022777 ) ) ;
#19685 = DIRECTION ( 'NONE',  ( 0.9934404589540162256, 0.1135548637187060589, -0.01346653032743021922 ) ) ;
#19686 = CARTESIAN_POINT ( 'NONE',  ( 78.05646167423948611, 75.18463598142704996, 4.911928902550189768 ) ) ;
#19687 = LINE ( 'NONE', #1796, #13350 ) ;
#19688 = EDGE_LOOP ( 'NONE', ( #21011, #18631, #10888, #13440, #11875 ) ) ;
#19689 = CARTESIAN_POINT ( 'NONE',  ( 12.25812685601325214, 187.6818734834393467, 322.9715098129762509 ) ) ;
#19690 = CARTESIAN_POINT ( 'NONE',  ( 0.000000000000000000, 0.000000000000000000, 0.000000000000000000 ) ) ;
#19691 = CARTESIAN_POINT ( 'NONE',  ( -37.32293697913370778, 166.0855081542887319, 269.1292477970816321 ) ) ;
#19692 = EDGE_CURVE ( 'NONE', #1018, #724, #15137, .T. ) ;
#19693 = VECTOR ( 'NONE', #11353, 999.9999999999998863 ) ;
#19694 = DIRECTION ( 'NONE',  ( -0.01292394549866741384, -0.005513023399720269613, -0.9999012842304692006 ) ) ;
#19695 = SURFACE_SIDE_STYLE ('',( #5585 ) ) ;
#19696 = CARTESIAN_POINT ( 'NONE',  ( -90.41664810497505300, 79.20851322806753103, 29.13399567714558103 ) ) ;
#19697 = DIRECTION ( 'NONE',  ( -0.01292414190464131508, -1.902755938799530474E-22, -0.9999164797902017066 ) ) ;
#19698 = ORIENTED_EDGE ( 'NONE', *, *, #15011, .F. ) ;
#19699 = DIRECTION ( 'NONE',  ( 0.8981428216242032248, 0.000000000000000000, 0.4397038457472424167 ) ) ;
#19700 = DIRECTION ( 'NONE',  ( 0.01292394549866743465, 0.005513023399721021615, 0.9999012842304692006 ) ) ;
#19701 = CARTESIAN_POINT ( 'NONE',  ( -15.52316384508689495, 177.7875914134558002, 315.5629757591011639 ) ) ;
#19702 = ORIENTED_EDGE ( 'NONE', *, *, #22444, .F. ) ;
#19703 = EDGE_LOOP ( 'NONE', ( #9648, #7628, #15557, #12255, #4430, #9086, #17321, #499 ) ) ;
#19704 = DIRECTION ( 'NONE',  ( 0.9999164797902015955, 6.965998958219364448E-18, -0.01292414190464157182 ) ) ;
#19705 = EDGE_CURVE ( 'NONE', #20838, #7432, #11144, .T. ) ;
#19706 = ORIENTED_EDGE ( 'NONE', *, *, #16286, .F. ) ;
#19707 = CIRCLE ( 'NONE', #18632, 3.399999999999986144 ) ;
#19708 = CARTESIAN_POINT ( 'NONE',  ( 12.06934323283736532, 188.4384883516733566, 306.8148419804898026 ) ) ;
#19709 = ADVANCED_FACE ( 'NONE', ( #17295 ), #17375, .F. ) ;
#19710 = ORIENTED_EDGE ( 'NONE', *, *, #14574, .F. ) ;
#19711 = DIRECTION ( 'NONE',  ( -0.000000000000000000, -1.000000000000000000, 0.000000000000000000 ) ) ;
#19712 = CARTESIAN_POINT ( 'NONE',  ( -10.85975448567659463, 163.0086244145724379, 126.9834806368866111 ) ) ;
#19713 = ORIENTED_EDGE ( 'NONE', *, *, #16556, .F. ) ;
#19714 = AXIS2_PLACEMENT_3D ( 'NONE', #957, #4602, #4700 ) ;
#19715 = EDGE_CURVE ( 'NONE', #168, #10199, #7463, .T. ) ;
#19716 = ORIENTED_EDGE ( 'NONE', *, *, #1952, .F. ) ;
#19717 = CARTESIAN_POINT ( 'NONE',  ( 5.149300590115022835, 70.80384757729338219, -98.24794683011701579 ) ) ;
#19718 = EDGE_CURVE ( 'NONE', #2916, #3937, #12978, .T. ) ;
#19719 = DIRECTION ( 'NONE',  ( -0.000000000000000000, -1.000000000000000000, -0.000000000000000000 ) ) ;
#19720 = ORIENTED_EDGE ( 'NONE', *, *, #9670, .T. ) ;
#19721 = CARTESIAN_POINT ( 'NONE',  ( -68.60435330951924016, 89.65606824129204711, 68.66099709659675909 ) ) ;
#19722 = CARTESIAN_POINT ( 'NONE',  ( 0.000000000000000000, 45.00000000000000000, 0.000000000000000000 ) ) ;
#19723 = DIRECTION ( 'NONE',  ( 7.125109674403837105E-05, -0.9999848031710252272, 0.005512562950847867821 ) ) ;
#19724 = DIRECTION ( 'NONE',  ( 0.3102455404053333088, 0.9506564598521396459, 0.000000000000000000 ) ) ;
#19725 = AXIS2_PLACEMENT_3D ( 'NONE', #22304, #13620, #4861 ) ;
#19726 = ORIENTED_EDGE ( 'NONE', *, *, #5846, .F. ) ;
#19727 = CARTESIAN_POINT ( 'NONE',  ( 50.34270678259964882, 126.1473026246199254, 26.19146026598277643 ) ) ;
#19728 = CARTESIAN_POINT ( 'NONE',  ( 68.31397436809166379, 127.4153035195791119, 255.9758934117053570 ) ) ;
#19729 = ADVANCED_FACE ( 'NONE', ( #22307 ), #13625, .F. ) ;
#19730 = ORIENTED_EDGE ( 'NONE', *, *, #11683, .T. ) ;
#19731 = EDGE_CURVE ( 'NONE', #16051, #11842, #1959, .T. ) ;
#19732 = CIRCLE ( 'NONE', #9851, 10.99999999999999289 ) ;
#19733 = FACE_OUTER_BOUND ( 'NONE', #6066, .T. ) ;
#19734 = CARTESIAN_POINT ( 'NONE',  ( -88.18706637290617323, 88.71869973106707619, 50.32066939225175872 ) ) ;
#19735 = EDGE_CURVE ( 'NONE', #19747, #12598, #10027, .T. ) ;
#19736 = APPLICATION_PROTOCOL_DEFINITION ( 'draft international standard', 'automotive_design', 1998, #22277 ) ;
#19737 = AXIS2_PLACEMENT_3D ( 'NONE', #8993, #14079, #7384 ) ;
#19738 = EDGE_LOOP ( 'NONE', ( #16495, #9317, #11495, #8038 ) ) ;
#19739 = LINE ( 'NONE', #16455, #16265 ) ;
#19740 = ORIENTED_EDGE ( 'NONE', *, *, #4813, .T. ) ;
#19741 = CARTESIAN_POINT ( 'NONE',  ( -154.0000000000000000, 1.999999999999998224, 53.76161406891259986 ) ) ;
#19742 = DIRECTION ( 'NONE',  ( 7.125109674364536131E-05, -0.9999848031710253382, 0.005512562950849705760 ) ) ;
#19743 = SURFACE_STYLE_FILL_AREA ( #17729 ) ;
#19744 = CARTESIAN_POINT ( 'NONE',  ( -106.2089377515398780, 72.00000000000000000, -28.62973177816246206 ) ) ;
#19745 = DIRECTION ( 'NONE',  ( 0.000000000000000000, 0.000000000000000000, -1.000000000000000000 ) ) ;
#19746 = CARTESIAN_POINT ( 'NONE',  ( 68.99891043397283852, 92.11203426037261011, -85.66888312730657162 ) ) ;
#19747 = VERTEX_POINT ( 'NONE', #19109 ) ;
#19748 = EDGE_CURVE ( 'NONE', #11124, #21547, #10398, .T. ) ;
#19749 = FACE_OUTER_BOUND ( 'NONE', #18657, .T. ) ;
#19750 = EDGE_LOOP ( 'NONE', ( #15369, #13559, #15920, #4952 ) ) ;
#19751 = CARTESIAN_POINT ( 'NONE',  ( -14.53254043310009358, 177.6255169206013989, 113.6379760112694584 ) ) ;
#19752 = PLANE ( 'NONE',  #8218 ) ;
#19753 = DIRECTION ( 'NONE',  ( 7.125109674160258889E-05, -0.9999848031710252272, 0.005512562950849897447 ) ) ;
#19754 = PLANE ( 'NONE',  #12162 ) ;
#19755 = AXIS2_PLACEMENT_3D ( 'NONE', #2307, #9308, #15064 ) ;
#19756 = CYLINDRICAL_SURFACE ( 'NONE', #10297, 2.499999999999988010 ) ;
#19757 = EDGE_LOOP ( 'NONE', ( #15653, #12541, #10389 ) ) ;
#19758 = DIRECTION ( 'NONE',  ( -0.01292394549866737914, -0.005513023399720295634, -0.9999012842304692006 ) ) ;
#19759 = ADVANCED_BREP_SHAPE_REPRESENTATION ( '', ( #17335, #6292 ), #1540 ) ;
#19760 = CIRCLE ( 'NONE', #15766, 4.200000000000005507 ) ;
#19761 = CARTESIAN_POINT ( 'NONE',  ( 41.15884018182899950, 107.0346074789500506, 92.70501406802365807 ) ) ;
#19762 = ORIENTED_EDGE ( 'NONE', *, *, #6832, .T. ) ;
#19763 = FACE_OUTER_BOUND ( 'NONE', #8057, .T. ) ;
#19764 = ORIENTED_EDGE ( 'NONE', *, *, #10367, .F. ) ;
#19765 = CARTESIAN_POINT ( 'NONE',  ( -105.0182314695230446, 70.09775045434527385, 32.72898861654373093 ) ) ;
#19766 = CARTESIAN_POINT ( 'NONE',  ( 12.84378735233264379, 190.4863133572641232, 307.8501959441126701 ) ) ;
#19767 = EDGE_CURVE ( 'NONE', #14285, #15416, #16970, .T. ) ;
#19768 = AXIS2_PLACEMENT_3D ( 'NONE', #19589, #7194, #2253 ) ;
#19770 = EDGE_LOOP ( 'NONE', ( #6352, #5934, #8719, #18840 ) ) ;
#19769 = ORIENTED_EDGE ( 'NONE', *, *, #19504, .F. ) ;
#19771 = CIRCLE ( 'NONE', #13929, 2.499999999999988010 ) ;
#19772 = CARTESIAN_POINT ( 'NONE',  ( 39.67545195212834130, 95.60340224533959486, -43.55612573487053396 ) ) ;
#19773 = CARTESIAN_POINT ( 'NONE',  ( -9.594263975657968402, 146.1660993649124123, 278.1580113407965769 ) ) ;
#19774 = CARTESIAN_POINT ( 'NONE',  ( -36.24790013166014546, 94.37751527644311977, -82.16087381192814121 ) ) ;
#19775 = LINE ( 'NONE', #11195, #12995 ) ;
#19776 = ADVANCED_FACE ( 'NONE', ( #4744 ), #5618, .T. ) ;
#19777 = CARTESIAN_POINT ( 'NONE',  ( -66.44851505496320954, 169.3797848675314128, -111.6488252521261160 ) ) ;
#19778 = CARTESIAN_POINT ( 'NONE',  ( 397.1141114976279027, 91.17157287525388654, 77.87414493559199968 ) ) ;
#19779 = CARTESIAN_POINT ( 'NONE',  ( 13.08424151692359061, 187.2836837763990161, 307.6956580856131040 ) ) ;
#19780 = DIRECTION ( 'NONE',  ( 1.000000000000000000, 0.000000000000000000, -0.000000000000000000 ) ) ;
#19781 = DIRECTION ( 'NONE',  ( -0.01292414190464131335, 0.000000000000000000, -0.9999164797902017066 ) ) ;
#19782 = CIRCLE ( 'NONE', #22665, 2.000000000000001776 ) ;
#19783 = CIRCLE ( 'NONE', #3664, 120.0000000000000142 ) ;
#19784 = LINE ( 'NONE', #2018, #6627 ) ;
#19785 = FACE_OUTER_BOUND ( 'NONE', #17917, .T. ) ;
#19786 = VERTEX_POINT ( 'NONE', #7172 ) ;
#19787 = CARTESIAN_POINT ( 'NONE',  ( 48.02316444802085016, 166.7281037598372961, 233.7692061953857774 ) ) ;
#19788 = ORIENTED_EDGE ( 'NONE', *, *, #16389, .F. ) ;
#19789 = EDGE_LOOP ( 'NONE', ( #4425, #4399, #13700, #10462 ) ) ;
#19790 = FACE_OUTER_BOUND ( 'NONE', #8212, .T. ) ;
#19791 = EDGE_CURVE ( 'NONE', #12496, #12459, #12605, .T. ) ;
#19792 = VECTOR ( 'NONE', #14476, 1000.000000000000114 ) ;
#19793 = ADVANCED_FACE ( 'NONE', ( #20945 ), #21397, .T. ) ;
#19794 = CARTESIAN_POINT ( 'NONE',  ( -4.315545553080798236, 70.55908004698144964, -99.47772690391983019 ) ) ;
#19795 = DIRECTION ( 'NONE',  ( -0.01292394549866632963, -0.005513023399716958026, -0.9999012842304692006 ) ) ;
#19796 = CARTESIAN_POINT ( 'NONE',  ( -38.69757710431294839, 94.02752048664900997, -82.47923521851862461 ) ) ;
#19797 = CARTESIAN_POINT ( 'NONE',  ( -89.40428028770215008, 69.94497429273697264, 63.29600751891009480 ) ) ;
#19798 = TOROIDAL_SURFACE ( 'NONE', #21287, 4.000000000000000000, 2.000000000000000000 ) ;
#19799 = ORIENTED_EDGE ( 'NONE', *, *, #11027, .T. ) ;
#19800 = B_SPLINE_CURVE_WITH_KNOTS ( 'NONE', 3,
 ( #7236, #5161, #15542, #8841, #1630, #18956, #22493, #12080, #17721, #19187, #15768, #3215, #10240, #20792, #19068, #13808 ),
 .UNSPECIFIED., .F., .F.,
 ( 4, 2, 2, 2, 2, 2, 2, 4 ),
 ( 0.000000000000000000, 0.0002817774770003779266, 0.0005635549540007558532, 0.001127109908001559194, 0.001690664862002362644, 0.002254219816003151348, 0.003381329724004707073, 0.004508439632006262798 ),
 .UNSPECIFIED. ) ;
#19801 = DIRECTION ( 'NONE',  ( 0.9999164797902015955, 6.965998958219364448E-18, -0.01292414190464157182 ) ) ;
#19802 = CARTESIAN_POINT ( 'NONE',  ( -41.08973838174756565, 106.8061942917681790, 71.47038841247318430 ) ) ;
#19803 = CIRCLE ( 'NONE', #15814, 7.499999999999992006 ) ;
#19804 = CARTESIAN_POINT ( 'NONE',  ( -47.41895600383423215, 106.0982379271226677, 200.0136222886318365 ) ) ;
#19805 = EDGE_LOOP ( 'NONE', ( #14746, #14267, #4739, #16002, #20278, #7970, #11309, #21905, #21710, #4927, #661, #600, #10253 ) ) ;
#19806 = CARTESIAN_POINT ( 'NONE',  ( -10.85624112972181621, 113.6998737626107641, 127.2553023597115498 ) ) ;
#19807 = ORIENTED_EDGE ( 'NONE', *, *, #9478, .F. ) ;
#19808 = CARTESIAN_POINT ( 'NONE',  ( 2.779577622087289868, 1.185696463474356088, 215.0506773825053983 ) ) ;
#19809 = PRODUCT_DEFINITION_FORMATION_WITH_SPECIFIED_SOURCE ( 'ANY', '', #14902, .NOT_KNOWN. ) ;
#19810 = CARTESIAN_POINT ( 'NONE',  ( 90.90343663577486666, 80.03933989046612396, -31.72203358726163103 ) ) ;
#19811 = CARTESIAN_POINT ( 'NONE',  ( 105.4334892372614405, 77.12912189496645965, -31.36525700924962834 ) ) ;
#19812 = AXIS2_PLACEMENT_3D ( 'NONE', #2495, #21985, #7994 ) ;
#19813 = CARTESIAN_POINT ( 'NONE',  ( -92.43457499998876870, 79.82103140525724427, 31.19724316448927226 ) ) ;
#19814 = CARTESIAN_POINT ( 'NONE',  ( -162.0000000000000000, 0.000000000000000000, 10.00000000000001776 ) ) ;
#19815 = ORIENTED_EDGE ( 'NONE', *, *, #7112, .F. ) ;
#19816 = CARTESIAN_POINT ( 'NONE',  ( -13.89421726780587996, 325.7902730365928505, 330.8534925327304563 ) ) ;
#19817 = FACE_OUTER_BOUND ( 'NONE', #12583, .T. ) ;
#19818 = CARTESIAN_POINT ( 'NONE',  ( -13.66360798539897381, 182.8253664500271043, 319.2043023236377621 ) ) ;
#19819 = ORIENTED_EDGE ( 'NONE', *, *, #5534, .T. ) ;
#19820 = CIRCLE ( 'NONE', #9938, 3.099999999999998757 ) ;
#19821 = ORIENTED_EDGE ( 'NONE', *, *, #1301, .T. ) ;
#19822 = CIRCLE ( 'NONE', #2241, 7.500000000000002665 ) ;
#19823 = DIRECTION ( 'NONE',  ( 7.125109674364534776E-05, -0.9999848031710252272, 0.005512562950849704893 ) ) ;
#19824 = VECTOR ( 'NONE', #1104, 999.9999999999998863 ) ;
#19825 = DIRECTION ( 'NONE',  ( 7.176269450075763143E-19, -1.000000000000000000, 5.550596000020002074E-17 ) ) ;
#19826 = AXIS2_PLACEMENT_3D ( 'NONE', #11883, #8307, #5929 ) ;
#19827 = ITEM_DEFINED_TRANSFORMATION ( 'NONE', 'NONE', #3668,  #6292 ) ;
#19828 = ORIENTED_EDGE ( 'NONE', *, *, #18410, .F. ) ;
#19829 = DIRECTION ( 'NONE',  ( -0.004829518060344538052, -0.03945926991566315462, -0.9992095084480668854 ) ) ;
#19830 = DIRECTION ( 'NONE',  ( 0.9999164797902015955, 6.965998958219364448E-18, -0.01292414190464157182 ) ) ;
#19831 = ORIENTED_EDGE ( 'NONE', *, *, #17533, .T. ) ;
#19832 = EDGE_LOOP ( 'NONE', ( #18847, #5199, #21370 ) ) ;
#19833 = CYLINDRICAL_SURFACE ( 'NONE', #639, 7.921742784567035400 ) ;
#19834 = CIRCLE ( 'NONE', #9962, 10.99999999999999289 ) ;
#19835 = ORIENTED_EDGE ( 'NONE', *, *, #10529, .T. ) ;
#19836 = CARTESIAN_POINT ( 'NONE',  ( -4.880720251855715119, 321.6948272370410109, 320.3571455402721426 ) ) ;
#19837 = CARTESIAN_POINT ( 'NONE',  ( -67.11636521215302764, 90.33521852268984276, 68.08362892527694044 ) ) ;
#19838 = ORIENTED_EDGE ( 'NONE', *, *, #8715, .T. ) ;
#19839 = FACE_OUTER_BOUND ( 'NONE', #16470, .T. ) ;
#19840 = TOROIDAL_SURFACE ( 'NONE', #17690, 10.00000000000000178, 2.272904689641331188 ) ;
#19841 = CARTESIAN_POINT ( 'NONE',  ( -41.00454908889594918, 95.41939025383068440, -42.83076017402247260 ) ) ;
#19842 = CARTESIAN_POINT ( 'NONE',  ( -91.62437796271721879, 72.00000000000000000, -60.86849236629028326 ) ) ;
#19843 = B_SPLINE_CURVE_WITH_KNOTS ( 'NONE', 3,
 ( #2406, #16433, #4326, #13099, #18253, #9512 ),
 .UNSPECIFIED., .F., .F.,
 ( 4, 2, 4 ),
 ( 0.000000000000000000, 0.0009893175791656075909, 0.001978635158331215182 ),
 .UNSPECIFIED. ) ;
#19844 = ORIENTED_EDGE ( 'NONE', *, *, #7546, .F. ) ;
#19845 = CARTESIAN_POINT ( 'NONE',  ( 64.42478219708148401, 94.99786382055523859, -44.92356850672740620 ) ) ;
#19846 = AXIS2_PLACEMENT_3D ( 'NONE', #2264, #12839, #9265 ) ;
#19847 = CARTESIAN_POINT ( 'NONE',  ( -163.1715728752537871, -3.619427204118298386E-16, 8.828427124746209387 ) ) ;
#19848 = EDGE_LOOP ( 'NONE', ( #16116, #6895, #14991, #21265 ) ) ;
#19849 = ADVANCED_FACE ( 'NONE', ( #10955 ), #14085, .F. ) ;
#19850 = CARTESIAN_POINT ( 'NONE',  ( 67.23320572660466610, 192.1022009597330680, 17.60971032628828681 ) ) ;
#19851 = VECTOR ( 'NONE', #1762, 1000.000000000000000 ) ;
#19852 = CARTESIAN_POINT ( 'NONE',  ( -89.87294000974075914, 87.92385784770752366, 50.83317552486207092 ) ) ;
#19853 = EDGE_CURVE ( 'NONE', #19287, #12921, #5257, .T. ) ;
#19854 = VECTOR ( 'NONE', #11158, 1000.000000000000114 ) ;
#19856 = ORIENTED_EDGE ( 'NONE', *, *, #3932, .T. ) ;
#19855 = ORIENTED_EDGE ( 'NONE', *, *, #20990, .F. ) ;
#19857 = CYLINDRICAL_SURFACE ( 'NONE', #20112, 2.000000000000004441 ) ;
#19858 = CARTESIAN_POINT ( 'NONE',  ( 0.000000000000000000, 29.00000000000000711, 0.000000000000000000 ) ) ;
#19859 = VERTEX_POINT ( 'NONE', #3496 ) ;
#19860 = CARTESIAN_POINT ( 'NONE',  ( 1.247179693797900502, 45.00000000000000000, 96.49194029975444664 ) ) ;
#19861 = CIRCLE ( 'NONE', #17333, 4.000000000000002665 ) ;
#19862 = DIRECTION ( 'NONE',  ( -0.9506032891036972909, 0.3102281881984321754, 0.01057629388542893900 ) ) ;
#19863 = DIRECTION ( 'NONE',  ( -0.01292394549866737220, -0.005513023399725441691, -0.9999012842304692006 ) ) ;
#19864 = LINE ( 'NONE', #11043, #21415 ) ;
#19865 = EDGE_CURVE ( 'NONE', #9211, #3408, #8649, .T. ) ;
#19866 = ORIENTED_EDGE ( 'NONE', *, *, #7447, .F. ) ;
#19867 = DIRECTION ( 'NONE',  ( 0.000000000000000000, 1.000000000000000000, -0.000000000000000000 ) ) ;
#19868 = VERTEX_POINT ( 'NONE', #10511 ) ;
#19869 = DIRECTION ( 'NONE',  ( 0.9999164797902017066, 2.001050586450179871E-22, -0.01292414190464085018 ) ) ;
#19870 = EDGE_CURVE ( 'NONE', #11611, #11415, #5207, .T. ) ;
#19871 = DIRECTION ( 'NONE',  ( -0.01292394549866737914, -0.005513023399720295634, -0.9999012842304692006 ) ) ;
#19872 = FACE_OUTER_BOUND ( 'NONE', #18620, .T. ) ;
#19873 = CARTESIAN_POINT ( 'NONE',  ( -11.46885069223597853, 70.80384757729338219, -91.33151364841882014 ) ) ;
#19874 = VECTOR ( 'NONE', #8031, 1000.000000000000114 ) ;
#19875 = AXIS2_PLACEMENT_3D ( 'NONE', #17216, #4794, #13780 ) ;
#19876 = PLANE ( 'NONE',  #13622 ) ;
#19877 = EDGE_CURVE ( 'NONE', #5811, #5010, #15567, .T. ) ;
#19878 = ORIENTED_EDGE ( 'NONE', *, *, #9642, .F. ) ;
#19879 = CARTESIAN_POINT ( 'NONE',  ( 68.30941429790007646, 191.4143309225247549, 255.6230893828509352 ) ) ;
#19880 = FACE_OUTER_BOUND ( 'NONE', #21973, .T. ) ;
#19881 = CARTESIAN_POINT ( 'NONE',  ( 41.20572975695933593, 107.5148010522800064, 93.02654324256212703 ) ) ;
#19882 = ORIENTED_EDGE ( 'NONE', *, *, #16037, .T. ) ;
#19883 = CARTESIAN_POINT ( 'NONE',  ( -162.0000000000000000, 20.00000000000000000, 0.000000000000000000 ) ) ;
#19884 = CIRCLE ( 'NONE', #18801, 3.099999999999998757 ) ;
#19885 = EDGE_LOOP ( 'NONE', ( #11644, #8019, #14714, #11481, #14762, #19923, #19072, #19856, #15667, #4690, #15265, #16171 ) ) ;
#19886 = ORIENTED_EDGE ( 'NONE', *, *, #16193, .T. ) ;
#19887 = EDGE_CURVE ( 'NONE', #3811, #1319, #17024, .T. ) ;
#19888 = CARTESIAN_POINT ( 'NONE',  ( -80.72910506257878183, 75.13519840835959940, -4.023912070737448055 ) ) ;
#19889 = CARTESIAN_POINT ( 'NONE',  ( -88.16232390766455751, 88.13524946876771082, 53.00763616620414354 ) ) ;
#19890 = ADVANCED_FACE ( 'NONE', ( #8998 ), #5736, .F. ) ;
#19891 = LINE ( 'NONE', #9692, #17198 ) ;
#19892 = CONICAL_SURFACE ( 'NONE', #9650, 4.999999999999990230, 1.047197551196595855 ) ;
#19893 = EDGE_LOOP ( 'NONE', ( #9255, #14647, #21553, #15018 ) ) ;
#19894 = ORIENTED_EDGE ( 'NONE', *, *, #17652, .T. ) ;
#19895 = CIRCLE ( 'NONE', #9259, 6.250000000000000000 ) ;
#19896 = DIRECTION ( 'NONE',  ( 0.3101392564284313758, 0.9506461370142480494, -0.009250070373107145000 ) ) ;
#19897 = CARTESIAN_POINT ( 'NONE',  ( -89.71476837554281758, 79.66528429935017641, -28.24846625074281548 ) ) ;
#19898 = CARTESIAN_POINT ( 'NONE',  ( 5.149300590115022835, 81.19615242270661781, -98.24794683011701579 ) ) ;
#19899 = AXIS2_PLACEMENT_3D ( 'NONE', #8133, #2741, #15041 ) ;
#19900 = FACE_OUTER_BOUND ( 'NONE', #15248, .T. ) ;
#19901 = DIRECTION ( 'NONE',  ( 7.125109674143708543E-05, -0.9999848031710252272, 0.005512562950848880899 ) ) ;
#19902 = CARTESIAN_POINT ( 'NONE',  ( 19.71973137965292366, 182.8876731017876978, 312.3882680660079814 ) ) ;
#19903 = CARTESIAN_POINT ( 'NONE',  ( 92.94153934368185332, 77.13727434530989058, 28.81475843614362375 ) ) ;
#19904 = DIRECTION ( 'NONE',  ( 7.125109674143708543E-05, -0.9999848031710252272, 0.005512562950848880899 ) ) ;
#19905 = EDGE_CURVE ( 'NONE', #16093, #1720, #19775, .T. ) ;
#19906 = VECTOR ( 'NONE', #11441, 1000.000000000000114 ) ;
#19907 = AXIS2_PLACEMENT_3D ( 'NONE', #3515, #15954, #7419 ) ;
#19908 = DIRECTION ( 'NONE',  ( 7.125109674403277385E-05, -0.9999848031710253382, 0.005512562950848281552 ) ) ;
#19909 = CARTESIAN_POINT ( 'NONE',  ( 24.26373134495293726, 168.9906716024700017, 301.3204665990833178 ) ) ;
#19910 = ORIENTED_EDGE ( 'NONE', *, *, #14796, .F. ) ;
#19911 = CARTESIAN_POINT ( 'NONE',  ( 157.5176307659770885, 2.000000000000000000, -60.94675664190840081 ) ) ;
#19912 = ORIENTED_EDGE ( 'NONE', *, *, #12170, .F. ) ;
#19913 = EDGE_LOOP ( 'NONE', ( #15130, #2176, #22118 ) ) ;
#19914 = ADVANCED_FACE ( 'NONE', ( #5893 ), #2222, .F. ) ;
#19915 = CARTESIAN_POINT ( 'NONE',  ( 42.65965783573783909, 106.8159614793892018, 70.39661456005998730 ) ) ;
#19916 = ADVANCED_FACE ( 'NONE', ( #7515 ), #22474, .T. ) ;
#19917 = CIRCLE ( 'NONE', #149, 93.00000000000001421 ) ;
#19918 = CARTESIAN_POINT ( 'NONE',  ( -90.39220665717816416, 70.86425073819692955, 61.14263641236500035 ) ) ;
#19919 = CIRCLE ( 'NONE', #11884, 78.99999999999998579 ) ;
#19920 = CIRCLE ( 'NONE', #21747, 2.000000000000001332 ) ;
#19921 = CARTESIAN_POINT ( 'NONE',  ( -12.81536461602102683, 326.2504838843369726, 414.3222871145668478 ) ) ;
#19922 = LINE ( 'NONE', #4191, #5979 ) ;
#19923 = ORIENTED_EDGE ( 'NONE', *, *, #7824, .T. ) ;
#19924 = DIRECTION ( 'NONE',  ( 0.9999164797902015955, 6.965998958219364448E-18, -0.01292414190464157182 ) ) ;
#19925 = DIRECTION ( 'NONE',  ( -0.2423871446253842432, -0.0001816599914484795519, 0.9701795911685635598 ) ) ;
#19926 = CARTESIAN_POINT ( 'NONE',  ( 89.90288769592241636, 96.48106732636601635, -63.38356668362104784 ) ) ;
#19927 = CARTESIAN_POINT ( 'NONE',  ( 3.872354045398203937, 166.6517708494369856, 299.5967279023338392 ) ) ;
#19928 = FACE_OUTER_BOUND ( 'NONE', #17378, .T. ) ;
#19929 = EDGE_CURVE ( 'NONE', #9560, #198, #12471, .T. ) ;
#19930 = CARTESIAN_POINT ( 'NONE',  ( -9.687524877350609742, 187.7773076241416277, 321.1696142754236121 ) ) ;
#19931 = EDGE_CURVE ( 'NONE', #13755, #17081, #513, .T. ) ;
#19932 = CARTESIAN_POINT ( 'NONE',  ( -90.41742102548464288, 80.31838830481380853, 32.51148913194521839 ) ) ;
#19933 = CARTESIAN_POINT ( 'NONE',  ( -1.163172771417702700, 81.97459999999998104, -89.99248318111824574 ) ) ;
#19934 = VECTOR ( 'NONE', #15640, 1000.000000000000227 ) ;
#19935 = ORIENTED_EDGE ( 'NONE', *, *, #9226, .T. ) ;
#19936 = CARTESIAN_POINT ( 'NONE',  ( 50.79397376011281295, 189.4876967392748384, -93.64401692289283119 ) ) ;
#19937 = DIRECTION ( 'NONE',  ( 0.7938906895485154935, -0.003295407061475230052, -0.6080515712836220832 ) ) ;
#19938 = CARTESIAN_POINT ( 'NONE',  ( -9.427729116192457681, 184.7790183205190431, 305.3034345195356991 ) ) ;
#19939 = ORIENTED_EDGE ( 'NONE', *, *, #21082, .F. ) ;
#19940 = AXIS2_PLACEMENT_3D ( 'NONE', #14859, #12893, #5637 ) ;
#19941 = ORIENTED_EDGE ( 'NONE', *, *, #4092, .F. ) ;
#19942 = CIRCLE ( 'NONE', #6389, 2.499999999999988010 ) ;
#19943 = CARTESIAN_POINT ( 'NONE',  ( 11.35084583594941066, 176.0618768581043980, 299.4481834837243355 ) ) ;
#19944 = APPLICATION_CONTEXT ( 'automotive_design' ) ;
#19945 = DIRECTION ( 'NONE',  ( 0.9999164797902015955, 6.965998958219364448E-18, -0.01292414190464157182 ) ) ;
#19946 = ITEM_DEFINED_TRANSFORMATION ( 'NONE', 'NONE', #22345,  #6292 ) ;
#19947 = AXIS2_PLACEMENT_3D ( 'NONE', #1475, #15503, #22454 ) ;
#19948 = DIRECTION ( 'NONE',  ( 0.9999164797902015955, 2.001050586450177050E-22, -0.01292414190464223796 ) ) ;
#19949 = DIRECTION ( 'NONE',  ( -0.01292394549866632963, -0.005513023399716958026, -0.9999012842304692006 ) ) ;
#19950 = ORIENTED_EDGE ( 'NONE', *, *, #10461, .T. ) ;
#19951 = CIRCLE ( 'NONE', #19597, 110.1134477342067157 ) ;
#19952 = EDGE_LOOP ( 'NONE', ( #1939, #12452, #21486, #5525 ) ) ;
#19953 = AXIS2_PLACEMENT_3D ( 'NONE', #5244, #12289, #15511 ) ;
#19954 = DIRECTION ( 'NONE',  ( -0.7912924530843117310, 0.6113994113550571541, 0.006856638134102506846 ) ) ;
#19955 = EDGE_CURVE ( 'NONE', #8567, #14769, #11077, .T. ) ;
#19956 = CARTESIAN_POINT ( 'NONE',  ( -15.10609485879404801, 178.5662836768142654, 311.3009205210422010 ) ) ;
#19957 = VERTEX_POINT ( 'NONE', #19898 ) ;
#19958 = PLANE ( 'NONE',  #8153 ) ;
#19959 = ORIENTED_EDGE ( 'NONE', *, *, #451, .F. ) ;
#19960 = DIRECTION ( 'NONE',  ( 7.125109674081160920E-05, -0.9999848031710253382, 0.005512562950849312846 ) ) ;
#19961 = FACE_OUTER_BOUND ( 'NONE', #13483, .T. ) ;
#19962 = CARTESIAN_POINT ( 'NONE',  ( 23.31673526217817027, 141.4150907639734385, 256.4803039161023435 ) ) ;
#19963 = ORIENTED_EDGE ( 'NONE', *, *, #10767, .F. ) ;
#19964 = LINE ( 'NONE', #4457, #13789 ) ;
#19965 =( BOUNDED_SURFACE ( )  B_SPLINE_SURFACE ( 1, 3, ( 
 ( #13953, #14316, #6931, #12362 ),
 ( #8886, #16157, #17881, #19229 ) ),
 .UNSPECIFIED., .F., .F., .T. ) 
 B_SPLINE_SURFACE_WITH_KNOTS ( ( 2, 2 ),
 ( 4, 4 ),
 ( 0.000000000000000000, 1.000000000000000000 ),
 ( 0.000000000000000000, 1.000000000000000000 ),
 .UNSPECIFIED. ) 
 GEOMETRIC_REPRESENTATION_ITEM ( )  RATIONAL_B_SPLINE_SURFACE ( (
 ( 1.000000000000000000, 0.9946110163663458570, 0.9946110163663458570, 1.000000000000000000),
 ( 1.000000000000000000, 0.9946110163663458570, 0.9946110163663458570, 1.000000000000000000) ) ) 
 REPRESENTATION_ITEM ( '' )  SURFACE ( )  );
#19966 = COLOUR_RGB ( '', 0.66274510, 0.83137255, 0.94901961) ;
#19967 = CARTESIAN_POINT ( 'NONE',  ( 1.141353067861252013, 81.64298031427460955, -80.61740134152157111 ) ) ;
#19968 = VERTEX_POINT ( 'NONE', #21832 ) ;
#19969 = VECTOR ( 'NONE', #18823, 1000.000000000000114 ) ;
#19970 = DIRECTION ( 'NONE',  ( -2.459148776294495979E-24, 1.000000000000000000, -1.902597020224326827E-22 ) ) ;
#19971 = CARTESIAN_POINT ( 'NONE',  ( -89.76563352250762762, 88.05638224443494266, 50.75096294400219676 ) ) ;
#19972 = DIRECTION ( 'NONE',  ( -0.01111515896966808192, -0.01944631716101971608, -0.9997491155234656812 ) ) ;
#19973 = VERTEX_POINT ( 'NONE', #4168 ) ;
#19974 = CARTESIAN_POINT ( 'NONE',  ( -51.29282874781860357, 111.0349699797280181, -46.46914343950034265 ) ) ;
#19975 = ORIENTED_EDGE ( 'NONE', *, *, #21978, .F. ) ;
#19976 = DIRECTION ( 'NONE',  ( 0.01292394549866738955, 0.005513023399720468239, 0.9999012842304693116 ) ) ;
#19977 = LINE ( 'NONE', #13456, #20985 ) ;
#19978 = EDGE_LOOP ( 'NONE', ( #3144, #13447, #14697, #6837 ) ) ;
#19979 = AXIS2_PLACEMENT_3D ( 'NONE', #6885, #22374, #3451 ) ;
#19980 = CYLINDRICAL_SURFACE ( 'NONE', #20742, 2.000000000000003997 ) ;
#19981 = PRODUCT_DEFINITION_SHAPE ( 'NONE', 'NONE',  #7492 ) ;
#19982 = DIRECTION ( 'NONE',  ( 0.9999164797902015955, 2.001050586498092550E-22, -0.01292414190464117457 ) ) ;
#19983 = ORIENTED_EDGE ( 'NONE', *, *, #21764, .T. ) ;
#19984 = CARTESIAN_POINT ( 'NONE',  ( 34.02121088943146532, 93.60248310457335208, -83.02802698561426098 ) ) ;
#19985 = FACE_OUTER_BOUND ( 'NONE', #6711, .T. ) ;
#19986 = ORIENTED_EDGE ( 'NONE', *, *, #11600, .T. ) ;
#19987 = FACE_OUTER_BOUND ( 'NONE', #4622, .T. ) ;
#19988 = PLANE ( 'NONE',  #18846 ) ;
#19989 = DIRECTION ( 'NONE',  ( -0.01292394549866728373, -0.005513023399720296501, -0.9999012842304693116 ) ) ;
#19990 = CARTESIAN_POINT ( 'NONE',  ( -38.81891740251079170, 107.5014370005211504, 91.63662627299856922 ) ) ;
#19991 = ADVANCED_FACE ( 'NONE', ( #18208 ), #2455, .F. ) ;
#19992 = PLANE ( 'NONE',  #12962 ) ;
#19993 = PRESENTATION_STYLE_ASSIGNMENT (( #1993 ) ) ;
#19994 = CARTESIAN_POINT ( 'NONE',  ( 0.000000000000000000, 25.00000000000000000, 0.000000000000000000 ) ) ;
#19995 = ORIENTED_EDGE ( 'NONE', *, *, #1064, .T. ) ;
#19996 = DIRECTION ( 'NONE',  ( 7.125109674160325297E-05, -0.9999848031710252272, 0.005512562950849327591 ) ) ;
#19997 = ORIENTED_EDGE ( 'NONE', *, *, #7824, .F. ) ;
#19998 = AXIS2_PLACEMENT_3D ( 'NONE', #3355, #5292, #13820 ) ;
#19999 = EDGE_LOOP ( 'NONE', ( #1503, #15325, #16573, #10195 ) ) ;
#20000 = CARTESIAN_POINT ( 'NONE',  ( -80.59137632606918089, 75.13524200571961842, 6.109821417268855193 ) ) ;
#20001 = ADVANCED_FACE ( 'NONE', ( #13148 ), #11413, .T. ) ;
#20002 = CARTESIAN_POINT ( 'NONE',  ( -90.16287545800051362, 87.20002246365963572, 51.27670327837432040 ) ) ;
#20003 = EDGE_CURVE ( 'NONE', #10714, #11266, #18145, .T. ) ;
#20005 = VERTEX_POINT ( 'NONE', #1077 ) ;
#20004 = VERTEX_POINT ( 'NONE', #2900 ) ;
#20006 = EDGE_CURVE ( 'NONE', #22043, #17825, #22313, .T. ) ;
#20007 = DIRECTION ( 'NONE',  ( 7.125109674161246868E-05, -0.9999848031710252272, 0.005512562950850154186 ) ) ;
#20008 = CARTESIAN_POINT ( 'NONE',  ( 1.364373935098378649E-14, 105.0000000000000000, -9.836450281572198869E-15 ) ) ;
#20009 = ORIENTED_EDGE ( 'NONE', *, *, #16872, .T. ) ;
#20010 = CARTESIAN_POINT ( 'NONE',  ( -90.05353287048657762, 71.28481833429248127, 60.66482926606789050 ) ) ;
#20011 = DIRECTION ( 'NONE',  ( 0.000000000000000000, 1.000000000000000000, 0.000000000000000000 ) ) ;
#20012 = ORIENTED_EDGE ( 'NONE', *, *, #2050, .F. ) ;
#20013 = CARTESIAN_POINT ( 'NONE',  ( -10.02941182916328167, 187.9619130446263000, 308.1597555601239833 ) ) ;
#20014 = CIRCLE ( 'NONE', #10133, 7.000000000000021316 ) ;
#20015 = DIRECTION ( 'NONE',  ( -0.9999164797902017066, -2.001050586450178931E-22, 0.01292414190464131508 ) ) ;
#20016 = CARTESIAN_POINT ( 'NONE',  ( 19.77978298930075240, 183.7162053505926735, 313.0775227943956338 ) ) ;
#20017 = CARTESIAN_POINT ( 'NONE',  ( -50.59241450076314806, 108.3707227317548529, -45.51087538574414992 ) ) ;
#20018 = EDGE_CURVE ( 'NONE', #8794, #21267, #18539, .T. ) ;
#20019 = EDGE_CURVE ( 'NONE', #2375, #13612, #20664, .T. ) ;
#20020 = CARTESIAN_POINT ( 'NONE',  ( -10.85340889862633595, 73.95047783656255547, 127.4744267370078177 ) ) ;
#20021 = VERTEX_POINT ( 'NONE', #13821 ) ;
#20022 =( NAMED_UNIT ( * ) SI_UNIT ( $, .STERADIAN. ) SOLID_ANGLE_UNIT ( ) );
#20023 = EDGE_CURVE ( 'NONE', #6117, #16990, #13594, .T. ) ;
#20024 = B_SPLINE_CURVE_WITH_KNOTS ( 'NONE', 3,
 ( #5074, #12107, #10597, #7040, #1872, #3696, #17751, #17619 ),
 .UNSPECIFIED., .F., .F.,
 ( 4, 2, 2, 4 ),
 ( 0.002921157996827033858, 0.003648658589483258583, 0.004376159182139483309, 0.005831160367451867707 ),
 .UNSPECIFIED. ) ;
#20025 = DIRECTION ( 'NONE',  ( -0.9934404589540162256, -0.1135548637187056842, 0.01346653032743081423 ) ) ;
#20026 = DIRECTION ( 'NONE',  ( 0.01292394549866740169, 0.005513023399721125699, 0.9999012842304692006 ) ) ;
#20027 = ORIENTED_EDGE ( 'NONE', *, *, #15175, .T. ) ;
#20028 = CARTESIAN_POINT ( 'NONE',  ( -13.92298191476773894, 185.7071742144165398, 276.7194026170014922 ) ) ;
#20029 = ORIENTED_EDGE ( 'NONE', *, *, #11629, .T. ) ;
#20030 = ORIENTED_EDGE ( 'NONE', *, *, #21205, .T. ) ;
#20031 = ADVANCED_FACE ( 'NONE', ( #10145 ), #14480, .T. ) ;
#20032 = CARTESIAN_POINT ( 'NONE',  ( -25.02778843067846637, 55.00725983767637217, -132.4644698413844424 ) ) ;
#20033 = EDGE_CURVE ( 'NONE', #11275, #5453, #2799, .T. ) ;
#20034 = EDGE_CURVE ( 'NONE', #11300, #14017, #9441, .T. ) ;
#20035 = CARTESIAN_POINT ( 'NONE',  ( 75.17704036982685523, 75.01379216013427254, 0.6763203681379648113 ) ) ;
#20036 = CARTESIAN_POINT ( 'NONE',  ( -64.99457118636313169, 170.0000000000000284, 0.8400692238016805868 ) ) ;
#20037 = CARTESIAN_POINT ( 'NONE',  ( 73.92160891109067222, 75.01036581836726214, 0.4624093665085752813 ) ) ;
#20038 = DIRECTION ( 'NONE',  ( 0.01292394549866731669, 0.005513023399720593139, 0.9999012842304692006 ) ) ;
#20039 = FACE_BOUND ( 'NONE', #17264, .T. ) ;
#20040 = ORIENTED_EDGE ( 'NONE', *, *, #4507, .F. ) ;
#20041 = CARTESIAN_POINT ( 'NONE',  ( -68.73688910937089247, 91.46348651515936012, 85.87923151210681283 ) ) ;
#20042 = EDGE_LOOP ( 'NONE', ( #8174, #20415, #5270, #17551 ) ) ;
#20043 = DIRECTION ( 'NONE',  ( 1.000000000000000000, 0.000000000000000000, 0.000000000000000000 ) ) ;
#20044 = FACE_OUTER_BOUND ( 'NONE', #12393, .T. ) ;
#20045 = CARTESIAN_POINT ( 'NONE',  ( -39.06279898716250187, 108.3240682923980245, 72.76796811295301382 ) ) ;
#20046 = ADVANCED_FACE ( 'NONE', ( #4950 ), #14089, .T. ) ;
#20047 = FACE_OUTER_BOUND ( 'NONE', #15875, .T. ) ;
#20048 = CARTESIAN_POINT ( 'NONE',  ( -8.597624943140569798, 185.9633400538521641, 321.2390708565524733 ) ) ;
#20049 = DIRECTION ( 'NONE',  ( -0.000000000000000000, -1.000000000000000000, -0.000000000000000000 ) ) ;
#20050 = ORIENTED_EDGE ( 'NONE', *, *, #7843, .F. ) ;
#20051 = CARTESIAN_POINT ( 'NONE',  ( 49.78441085332420357, 189.4892230880255397, -93.35408680624050248 ) ) ;
#20052 = DIRECTION ( 'NONE',  ( 0.01292394549866743812, 0.005513023399720639109, 0.9999012842304693116 ) ) ;
#20053 = B_SPLINE_CURVE_WITH_KNOTS ( 'NONE', 3,
 ( #7708, #4479, #11510, #11620 ),
 .UNSPECIFIED., .F., .F.,
 ( 4, 4 ),
 ( 0.0002143831494830000448, 0.0008144042056134326562 ),
 .UNSPECIFIED. ) ;
#20054 = CARTESIAN_POINT ( 'NONE',  ( -14.30933683530841627, 181.6919563439129490, 311.0896036802490698 ) ) ;
#20055 = ORIENTED_EDGE ( 'NONE', *, *, #19630, .F. ) ;
#20056 = ORIENTED_EDGE ( 'NONE', *, *, #11788, .F. ) ;
#20057 = DIRECTION ( 'NONE',  ( -0.9999164797902015955, -6.965998958219364448E-18, 0.01292414190464157182 ) ) ;
#20058 = DIRECTION ( 'NONE',  ( 0.9999164797902017066, 2.001050586450178931E-22, -0.01292414190464131508 ) ) ;
#20059 = ADVANCED_FACE ( 'NONE', ( #10251 ), #17263, .F. ) ;
#20060 = AXIS2_PLACEMENT_3D ( 'NONE', #12778, #19753, #7596 ) ;
#20061 = CARTESIAN_POINT ( 'NONE',  ( -46.77041971896417749, 121.3072273804455250, 250.1896512867793945 ) ) ;
#20062 = DIRECTION ( 'NONE',  ( -0.01292394549866738782, -0.005513023399720468239, -0.9999012842304692006 ) ) ;
#20063 = ORIENTED_EDGE ( 'NONE', *, *, #8773, .T. ) ;
#20064 = VERTEX_POINT ( 'NONE', #6363 ) ;
#20065 = LINE ( 'NONE', #5714, #16429 ) ;
#20066 = ADVANCED_FACE ( 'NONE', ( #13383 ), #20359, .F. ) ;
#20067 = CARTESIAN_POINT ( 'NONE',  ( 20.96603472858061679, 99.74539563421257071, 74.61103786048234099 ) ) ;
#20068 = ORIENTED_EDGE ( 'NONE', *, *, #12432, .T. ) ;
#20069 = DIRECTION ( 'NONE',  ( -0.01292414190464023262, 0.000000000000000000, -0.9999164797902017066 ) ) ;
#20070 = CARTESIAN_POINT ( 'NONE',  ( -38.91889996795050166, 97.30032992285177329, 83.90116378639756078 ) ) ;
#20071 = CARTESIAN_POINT ( 'NONE',  ( -46.79669995352260514, 127.3639955235004777, 248.1563991125460973 ) ) ;
#20072 = CARTESIAN_POINT ( 'NONE',  ( 26.51110539662167298, 89.80349391623344957, 78.56384651380399475 ) ) ;
#20073 = ORIENTED_EDGE ( 'NONE', *, *, #15132, .F. ) ;
#20074 = LINE ( 'NONE', #2753, #2045 ) ;
#20075 = VECTOR ( 'NONE', #4931, 1000.000000000000114 ) ;
#20076 = CARTESIAN_POINT ( 'NONE',  ( -56.89103422957282419, 143.2573102595449654, 47.48611753646095224 ) ) ;
#20077 = VERTEX_POINT ( 'NONE', #10485 ) ;
#20078 = DIRECTION ( 'NONE',  ( -1.000000000000000000, 0.000000000000000000, 1.386679829960243376E-14 ) ) ;
#20079 = CARTESIAN_POINT ( 'NONE',  ( -89.32895058079316186, 89.12709046313005956, 51.43971369372994928 ) ) ;
#20080 = ADVANCED_FACE ( 'NONE', ( #19421 ), #17497, .T. ) ;
#20081 = EDGE_CURVE ( 'NONE', #18403, #2761, #6732, .T. ) ;
#20083 = ORIENTED_EDGE ( 'NONE', *, *, #5677, .T. ) ;
#20082 = ORIENTED_EDGE ( 'NONE', *, *, #20194, .F. ) ;
#20084 = FACE_OUTER_BOUND ( 'NONE', #5879, .T. ) ;
#20085 = DIRECTION ( 'NONE',  ( -0.1136178953597573593, 0.9935164314186355483, -0.004009283626633517415 ) ) ;
#20086 = CARTESIAN_POINT ( 'NONE',  ( 64.07473967894682687, 105.0000000000000000, -72.00569783435743432 ) ) ;
#20087 = PLANE ( 'NONE',  #16632 ) ;
#20088 = DIRECTION ( 'NONE',  ( -0.9934404589540162256, -0.1135548637187056842, 0.01346653032743081423 ) ) ;
#20089 = PRESENTATION_LAYER_ASSIGNMENT (  '', '', ( #4684 ) ) ;
#20090 = DIRECTION ( 'NONE',  ( 0.000000000000000000, 1.000000000000000000, -0.000000000000000000 ) ) ;
#20091 = ORIENTED_EDGE ( 'NONE', *, *, #19221, .T. ) ;
#20092 = CARTESIAN_POINT ( 'NONE',  ( -68.08232934915048418, 97.72070053556842595, 80.16590062297730412 ) ) ;
#20093 = ORIENTED_EDGE ( 'NONE', *, *, #9823, .F. ) ;
#20094 = CARTESIAN_POINT ( 'NONE',  ( -7.336909845677233477, 105.7000452102326591, 127.2629691083419203 ) ) ;
#20095 = DIRECTION ( 'NONE',  ( -0.01292414190463830014, 0.000000000000000000, -0.9999164797902017066 ) ) ;
#20096 = CARTESIAN_POINT ( 'NONE',  ( 79.99331838321626265, 102.0000000000000000, -1.033931352371318058 ) ) ;
#20097 = CARTESIAN_POINT ( 'NONE',  ( 9.942021649914385861, 113.6998737626107641, 126.9864802080949744 ) ) ;
#20098 = ORIENTED_EDGE ( 'NONE', *, *, #14559, .F. ) ;
#20099 = DIRECTION ( 'NONE',  ( -0.009188991635466050092, 0.7031977391749439921, -0.7109349492407662785 ) ) ;
#20100 = CARTESIAN_POINT ( 'NONE',  ( 79.99331838321626265, 54.99999999999999289, 3.966068647628676835 ) ) ;
#20101 = CARTESIAN_POINT ( 'NONE',  ( -1.163172771417704698, 45.00000000000000000, -89.99248318111816047 ) ) ;
#20102 = AXIS2_PLACEMENT_3D ( 'NONE', #7614, #4501, #18420 ) ;
#20103 = ORIENTED_EDGE ( 'NONE', *, *, #3594, .T. ) ;
#20104 = PLANE ( 'NONE',  #9085 ) ;
#20105 = VERTEX_POINT ( 'NONE', #16122 ) ;
#20106 = CARTESIAN_POINT ( 'NONE',  ( -82.60517719326530539, 75.10270664613311453, -3.349685274425296289 ) ) ;
#20107 = CARTESIAN_POINT ( 'NONE',  ( -90.14611826098273184, 88.22591548105474146, 52.97392334573774519 ) ) ;
#20108 = CARTESIAN_POINT ( 'NONE',  ( 50.34271970654513950, 126.1473081376433214, 26.19246016726700788 ) ) ;
#20109 = ORIENTED_EDGE ( 'NONE', *, *, #17136, .T. ) ;
#20110 = CARTESIAN_POINT ( 'NONE',  ( -66.71921353929309362, 98.29062372165722650, 79.57831125914253789 ) ) ;
#20111 = LINE ( 'NONE', #8062, #13169 ) ;
#20112 = AXIS2_PLACEMENT_3D ( 'NONE', #18274, #5849, #9662 ) ;
#20113 = CARTESIAN_POINT ( 'NONE',  ( -92.64101326278360204, 79.05197601643141070, -26.25411123107253530 ) ) ;
#20114 = CARTESIAN_POINT ( 'NONE',  ( 396.0414077195426898, 177.0000000000003695, -5.118922886994747401 ) ) ;
#20115 = ORIENTED_EDGE ( 'NONE', *, *, #6988, .T. ) ;
#20116 = LINE ( 'NONE', #19777, #384 ) ;
#20117 = CARTESIAN_POINT ( 'NONE',  ( -14.37471740060550118, 109.6998846769365628, 127.3137863664913425 ) ) ;
#20118 = CARTESIAN_POINT ( 'NONE',  ( 18.31812028490978861, 185.8289673428165543, 318.2867877985925134 ) ) ;
#20119 = CARTESIAN_POINT ( 'NONE',  ( 93.21002351426729149, 77.12912189496637438, 28.79774562292276840 ) ) ;
#20120 = PLANE ( 'NONE',  #15950 ) ;
#20121 = ADVANCED_FACE ( 'NONE', ( #17735 ), #8727, .T. ) ;
#20122 = PLANE ( 'NONE',  #4038 ) ;
#20123 = ORIENTED_EDGE ( 'NONE', *, *, #452, .T. ) ;
#20124 = B_SPLINE_CURVE_WITH_KNOTS ( 'NONE', 3,
 ( #8067, #21940, #22059, #22180, #18536, #20575, #11535, #6473, #1419, #20460, #11872, #4716, #11752, #18746, #18861, #8396, #6686, #15441 ),
 .UNSPECIFIED., .F., .F.,
 ( 4, 2, 2, 2, 2, 2, 2, 2, 4 ),
 ( -8.963567119963375336E-06, 0.0003869120770741988550, 0.0007827877212683610753, 0.001178663365462523241, 0.001574539009656685407, 0.001970414653850847790, 0.002366290298045010173, 0.002762165942239172122, 0.003158041586433334505 ),
 .UNSPECIFIED. ) ;
#20125 = CYLINDRICAL_SURFACE ( 'NONE', #18729, 10.00000000000000000 ) ;
#20126 = LINE ( 'NONE', #7866, #21302 ) ;
#20127 = ORIENTED_EDGE ( 'NONE', *, *, #14353, .F. ) ;
#20128 = DIRECTION ( 'NONE',  ( -0.01292394549866742424, -0.005513023399720750999, -0.9999012842304693116 ) ) ;
#20129 = CIRCLE ( 'NONE', #8395, 11.78759343285143224 ) ;
#20130 = ORIENTED_EDGE ( 'NONE', *, *, #15700, .T. ) ;
#20131 = DIRECTION ( 'NONE',  ( -2.449293598294706414E-16, -0.000000000000000000, -1.000000000000000000 ) ) ;
#20132 = CARTESIAN_POINT ( 'NONE',  ( -9.837386872088778489, 187.7736565290674662, 321.1595949917730763 ) ) ;
#20133 = ORIENTED_EDGE ( 'NONE', *, *, #22183, .F. ) ;
#20134 = AXIS2_PLACEMENT_3D ( 'NONE', #16111, #18054, #9530 ) ;
#20135 = ADVANCED_FACE ( 'NONE', ( #8853 ), #6905, .T. ) ;
#20136 = EDGE_LOOP ( 'NONE', ( #12794, #18531, #21494, #5794, #1268, #21961, #17845 ) ) ;
#20137 = EDGE_CURVE ( 'NONE', #16568, #12132, #1609, .T. ) ;
#20138 = FACE_OUTER_BOUND ( 'NONE', #15007, .T. ) ;
#20139 = CARTESIAN_POINT ( 'NONE',  ( 76.19828175484278177, 75.05963785504690122, 2.389257670094249164 ) ) ;
#20140 = CARTESIAN_POINT ( 'NONE',  ( 23.22230400743448442, 141.3748088146942621, 249.1743358663702566 ) ) ;
#20141 = CARTESIAN_POINT ( 'NONE',  ( 74.61645886759328050, 75.05117449683021391, 2.158817404397858297 ) ) ;
#20142 = CARTESIAN_POINT ( 'NONE',  ( -157.5176307659779411, 2.000000000000000000, -60.94675664190620523 ) ) ;
#20143 = ORIENTED_EDGE ( 'NONE', *, *, #14900, .T. ) ;
#20144 = CARTESIAN_POINT ( 'NONE',  ( 11.01344518422641805, 189.7760306036772704, 274.8985146619464786 ) ) ;
#20145 = DIRECTION ( 'NONE',  ( 0.001060663555083274368, -0.002015910208784305047, 0.9999974055460609801 ) ) ;
#20146 = CARTESIAN_POINT ( 'NONE',  ( -59.30749807291185505, 114.2358014486931808, 170.6782526301398661 ) ) ;
#20147 = LINE ( 'NONE', #16644, #912 ) ;
#20148 = AXIS2_PLACEMENT_3D ( 'NONE', #15386, #10310, #10092 ) ;
#20149 = CIRCLE ( 'NONE', #8415, 3.309500000000006992 ) ;
#20150 = EDGE_CURVE ( 'NONE', #2955, #3529, #254, .T. ) ;
#20151 = CARTESIAN_POINT ( 'NONE',  ( 89.97519728687149154, 79.29963411167463505, -29.42247391813773660 ) ) ;
#20152 = CARTESIAN_POINT ( 'NONE',  ( -8.553411222537889103, 185.9935125942876084, 321.2420807565750351 ) ) ;
#20153 = DIRECTION ( 'NONE',  ( -0.9232306267972774094, 0.000000000000000000, 0.3842462878721227826 ) ) ;
#20154 = VERTEX_POINT ( 'NONE', #21147 ) ;
#20155 = DIRECTION ( 'NONE',  ( 0.3101392564284315978, 0.9506461370142478273, -0.009250070373106959384 ) ) ;
#20156 = EDGE_LOOP ( 'NONE', ( #728, #4790, #3492, #13129 ) ) ;
#20157 = EDGE_CURVE ( 'NONE', #15668, #4798, #14275, .T. ) ;
#20158 = ORIENTED_EDGE ( 'NONE', *, *, #21407, .F. ) ;
#20159 = DIRECTION ( 'NONE',  ( -7.125109674403276030E-05, 0.9999848031710252272, -0.005512562950848280685 ) ) ;
#20160 = VECTOR ( 'NONE', #13544, 1000.000000000000227 ) ;
#20161 = CARTESIAN_POINT ( 'NONE',  ( -8.647491781698080970, 185.3224403731376810, 308.0171747953146451 ) ) ;
#20162 = ORIENTED_EDGE ( 'NONE', *, *, #5094, .T. ) ;
#20163 = VERTEX_POINT ( 'NONE', #21038 ) ;
#20164 = AXIS2_PLACEMENT_3D ( 'NONE', #6051, #4200, #657 ) ;
#20165 = PRODUCT ( 'Handle Handwheel Knob', 'Handle Handwheel Knob', '', ( #21359 ) ) ;
#20166 = AXIS2_PLACEMENT_3D ( 'NONE', #4051, #12930, #11078 ) ;
#20167 = FACE_OUTER_BOUND ( 'NONE', #19885, .T. ) ;
#20168 = EDGE_CURVE ( 'NONE', #984, #2805, #17852, .T. ) ;
#20169 = PRODUCT_DEFINITION_FORMATION_WITH_SPECIFIED_SOURCE ( 'ANY', '', #5355, .NOT_KNOWN. ) ;
#20170 = EDGE_CURVE ( 'NONE', #1018, #10488, #19919, .T. ) ;
#20171 = CARTESIAN_POINT ( 'NONE',  ( 0.000000000000000000, 0.000000000000000000, 0.000000000000000000 ) ) ;
#20172 = AXIS2_PLACEMENT_3D ( 'NONE', #22215, #1566, #22540 ) ;
#20173 = DIRECTION ( 'NONE',  ( -2.025474946048326158E-22, 1.000000000000000000, -1.876735158486679638E-22 ) ) ;
#20174 = VERTEX_POINT ( 'NONE', #143 ) ;
#20175 = CYLINDRICAL_SURFACE ( 'NONE', #906, 2.000000000000001332 ) ;
#20176 = CARTESIAN_POINT ( 'NONE',  ( 12.56180216312617226, 190.5919383268307286, 307.8320289183637897 ) ) ;
#20177 = CARTESIAN_POINT ( 'NONE',  ( -8.967245084563666424, 185.1109935582825869, 305.2095739818239508 ) ) ;
#20178 = ORIENTED_EDGE ( 'NONE', *, *, #13583, .F. ) ;
#20179 = DIRECTION ( 'NONE',  ( -0.01096700916508646859, 0.5290868411612599242, -0.8484968115555724388 ) ) ;
#20180 = DIRECTION ( 'NONE',  ( -0.01246513159389404414, -0.2641402835564772844, -0.9644037178988117409 ) ) ;
#20181 = DIRECTION ( 'NONE',  ( -0.01292414190463827932, 0.000000000000000000, -0.9999164797902018176 ) ) ;
#20182 = AXIS2_PLACEMENT_3D ( 'NONE', #5646, #12340, #7153 ) ;
#20183 = EDGE_LOOP ( 'NONE', ( #15075, #17, #4032 ) ) ;
#20184 = VECTOR ( 'NONE', #12161, 1000.000000000000114 ) ;
#20185 = EDGE_CURVE ( 'NONE', #1581, #11360, #13926, .T. ) ;
#20186 = DIRECTION ( 'NONE',  ( 7.125109674364534776E-05, -0.9999848031710252272, 0.005512562950849704893 ) ) ;
#20187 = AXIS2_PLACEMENT_3D ( 'NONE', #12405, #12300, #17578 ) ;
#20188 = VECTOR ( 'NONE', #4003, 1000.000000000000000 ) ;
#20189 = CARTESIAN_POINT ( 'NONE',  ( -22.66159625276162970, 324.6936785073799001, 307.5691494985305781 ) ) ;
#20190 = AXIS2_PLACEMENT_3D ( 'NONE', #20625, #17185, #20836 ) ;
#20191 = ORIENTED_EDGE ( 'NONE', *, *, #10949, .F. ) ;
#20192 = B_SPLINE_CURVE_WITH_KNOTS ( 'NONE', 3,
 ( #3711, #5545, #10850, #4164 ),
 .UNSPECIFIED., .F., .F.,
 ( 4, 4 ),
 ( 0.000000000000000000, 0.001506161017265817467 ),
 .UNSPECIFIED. ) ;
#20193 = DIRECTION ( 'NONE',  ( 0.01111468050521610164, -0.5103046645782707280, 0.8599218645824314722 ) ) ;
#20194 = EDGE_CURVE ( 'NONE', #14615, #3864, #21248, .T. ) ;
#20195 = CARTESIAN_POINT ( 'NONE',  ( -88.17377687331638469, 88.93069077600954131, 51.92116411951112553 ) ) ;
#20196 = EDGE_CURVE ( 'NONE', #20403, #11929, #21401, .T. ) ;
#20197 = CONTEXT_DEPENDENT_SHAPE_REPRESENTATION ( #304, #17470 ) ;
#20198 = VERTEX_POINT ( 'NONE', #3573 ) ;
#20199 = AXIS2_PLACEMENT_3D ( 'NONE', #19909, #981, #4180 ) ;
#20200 = CARTESIAN_POINT ( 'NONE',  ( 91.34851551837616057, 77.30892464375352802, -31.47853330177477460 ) ) ;
#20201 = DIRECTION ( 'NONE',  ( 0.009760756503427210282, -0.9999378516499566327, 0.005387065077606872227 ) ) ;
#20202 = LINE ( 'NONE', #16693, #1541 ) ;
#20203 =( GEOMETRIC_REPRESENTATION_CONTEXT ( 3 ) GLOBAL_UNCERTAINTY_ASSIGNED_CONTEXT ( ( #15056 ) ) GLOBAL_UNIT_ASSIGNED_CONTEXT ( ( #2065, #10567, #10907 ) ) REPRESENTATION_CONTEXT ( 'NONE', 'WORKASPACE' ) );
#20204 = LINE ( 'NONE', #4471, #1573 ) ;
#20205 = AXIS2_PLACEMENT_3D ( 'NONE', #20456, #3465, #19307 ) ;
#20206 = DIRECTION ( 'NONE',  ( 0.000000000000000000, 0.000000000000000000, 1.000000000000000000 ) ) ;
#20207 = DIRECTION ( 'NONE',  ( 7.125109674160258889E-05, -0.9999848031710252272, 0.005512562950849897447 ) ) ;
#20208 = DIRECTION ( 'NONE',  ( 7.125109674403277385E-05, -0.9999848031710253382, 0.005512562950848281552 ) ) ;
#20209 = ORIENTED_EDGE ( 'NONE', *, *, #1085, .F. ) ;
#20210 = CARTESIAN_POINT ( 'NONE',  ( 39.42082737383937996, 69.99999999999998579, -83.51645567887783272 ) ) ;
#20211 = CIRCLE ( 'NONE', #2622, 112.5000000000007105 ) ;
#20212 = ORIENTED_EDGE ( 'NONE', *, *, #7951, .F. ) ;
#20213 = CARTESIAN_POINT ( 'NONE',  ( -41.56623493000981284, 69.99999999999998579, -82.46967996629571473 ) ) ;
#20214 = DIRECTION ( 'NONE',  ( -2.775557561562888984E-15, 0.000000000000000000, 1.000000000000000000 ) ) ;
#20215 = CARTESIAN_POINT ( 'NONE',  ( 3.898201936395599532, 166.6627968962365287, 301.5965304707955852 ) ) ;
#20216 = FACE_OUTER_BOUND ( 'NONE', #16186, .T. ) ;
#20217 = ADVANCED_FACE ( 'NONE', ( #3356 ), #3471, .F. ) ;
#20218 = EDGE_CURVE ( 'NONE', #15083, #307, #8623, .T. ) ;
#20219 = CARTESIAN_POINT ( 'NONE',  ( -11.19153202869804353, 137.5572120012638777, 101.3144779797563189 ) ) ;
#20220 = DIRECTION ( 'NONE',  ( 0.000000000000000000, 0.000000000000000000, 1.000000000000000000 ) ) ;
#20221 = ADVANCED_FACE ( 'NONE', ( #22610, #12433, #20917 ), #5175, .F. ) ;
#20222 = DIRECTION ( 'NONE',  ( -0.01292414190464131335, -1.358703943142685684E-38, -0.9999164797902015955 ) ) ;
#20223 = ORIENTED_EDGE ( 'NONE', *, *, #18315, .F. ) ;
#20224 = CIRCLE ( 'NONE', #14391, 23.67057332475409126 ) ;
#20225 = CARTESIAN_POINT ( 'NONE',  ( 51.60019979106838406, 180.9901659820745294, 273.9681169626219344 ) ) ;
#20226 = DIRECTION ( 'NONE',  ( -5.440186201345785633E-18, -1.000000000000000000, -1.334940939666367878E-17 ) ) ;
#20227 = ORIENTED_EDGE ( 'NONE', *, *, #1671, .T. ) ;
#20228 = TOROIDAL_SURFACE ( 'NONE', #16235, 8.000000000000001776, 6.520833333333323267 ) ;
#20229 = ORIENTED_EDGE ( 'NONE', *, *, #13175, .T. ) ;
#20230 = CARTESIAN_POINT ( 'NONE',  ( 58.90710753996705762, 143.6018742220277318, 108.4936714818314840 ) ) ;
#20231 = CARTESIAN_POINT ( 'NONE',  ( -90.17115648626537450, 87.10657506226966973, 51.33342129164628886 ) ) ;
#20232 = AXIS2_PLACEMENT_3D ( 'NONE', #15967, #19699, #3967 ) ;
#20233 = DIRECTION ( 'NONE',  ( -0.01292414190464044772, -8.765831891243140473E-39, -0.9999164797902015955 ) ) ;
#20235 = VERTEX_POINT ( 'NONE', #5516 ) ;
#20234 = ORIENTED_EDGE ( 'NONE', *, *, #18229, .F. ) ;
#20236 = DIRECTION ( 'NONE',  ( 7.125109674364536131E-05, -0.9999848031710253382, 0.005512562950849705760 ) ) ;
#20237 = DIRECTION ( 'NONE',  ( 0.009760756503427876415, -0.9999378516499564107, 0.005387065077611007807 ) ) ;
#20238 = FACE_OUTER_BOUND ( 'NONE', #21874, .T. ) ;
#20239 = CIRCLE ( 'NONE', #446, 3.399999999999985700 ) ;
#20240 = CARTESIAN_POINT ( 'NONE',  ( 48.02316444802085016, 166.7281037598372961, 233.7692061953857774 ) ) ;
#20241 = AXIS2_PLACEMENT_3D ( 'NONE', #12401, #8688, #19037 ) ;
#20242 = TOROIDAL_SURFACE ( 'NONE', #1909, 10.00000000000000355, 2.000000000000000000 ) ;
#20243 = CARTESIAN_POINT ( 'NONE',  ( -36.89904403399447119, 94.47498387040556622, 83.88519491590665211 ) ) ;
#20244 = EDGE_LOOP ( 'NONE', ( #17056, #6835 ) ) ;
#20245 = DIRECTION ( 'NONE',  ( -0.9999164797902015955, -2.001050586450178695E-22, 0.01292414190464131335 ) ) ;
#20246 = LINE ( 'NONE', #17155, #11895 ) ;
#20247 = CARTESIAN_POINT ( 'NONE',  ( 18.75241981682919956, 183.8790985612903057, 320.1233202157981168 ) ) ;
#20248 = DIRECTION ( 'NONE',  ( 0.01292414190464131508, 0.000000000000000000, 0.9999164797902017066 ) ) ;
#20249 = ADVANCED_FACE ( 'NONE', ( #14962 ), #17954, .F. ) ;
#20250 = CARTESIAN_POINT ( 'NONE',  ( -49.07907105527128522, 106.8061942917681790, 71.57365230629126529 ) ) ;
#20251 = ORIENTED_EDGE ( 'NONE', *, *, #11782, .F. ) ;
#20252 = CIRCLE ( 'NONE', #19514, 4.199999999999997513 ) ;
#20253 = APPLICATION_CONTEXT ( 'automotive_design' ) ;
#20254 = CARTESIAN_POINT ( 'NONE',  ( 43.08423624159371457, 94.48610424851698042, 82.84014869562156491 ) ) ;
#20255 = DIRECTION ( 'NONE',  ( 0.9999164797902017066, 2.001050586450178931E-22, -0.01292414190464131508 ) ) ;
#20256 = EDGE_LOOP ( 'NONE', ( #6179, #11763, #21511, #17164 ) ) ;
#20258 = CARTESIAN_POINT ( 'NONE',  ( 0.000000000000000000, 45.00000000000000711, 0.000000000000000000 ) ) ;
#20257 = AXIS2_PLACEMENT_3D ( 'NONE', #1670, #1886, #21063 ) ;
#20259 = EDGE_LOOP ( 'NONE', ( #10242, #1596, #1369 ) ) ;
#20260 = ORIENTED_EDGE ( 'NONE', *, *, #18923, .F. ) ;
#20261 = AXIS2_PLACEMENT_3D ( 'NONE', #15845, #88, #2489 ) ;
#20262 = DIRECTION ( 'NONE',  ( 0.01292394549866729934, 0.005513023399719703226, 0.9999012842304692006 ) ) ;
#20263 = ORIENTED_EDGE ( 'NONE', *, *, #6962, .F. ) ;
#20264 = ORIENTED_EDGE ( 'NONE', *, *, #16162, .T. ) ;
#20265 = CIRCLE ( 'NONE', #10383, 4.000000000000006217 ) ;
#20266 = CARTESIAN_POINT ( 'NONE',  ( -55.98629706596215527, 114.1919480473872852, 162.6802715674982664 ) ) ;
#20267 = CARTESIAN_POINT ( 'NONE',  ( 74.89842485966445906, 75.00001493645878270, -0.6274227567034913466 ) ) ;
#20268 = DIRECTION ( 'NONE',  ( 0.9999164797902017066, 6.965998958219365988E-18, -0.01292414190464157356 ) ) ;
#20269 = CARTESIAN_POINT ( 'NONE',  ( 85.00589227782222679, 75.07622562672395361, 2.721739690384933130 ) ) ;
#20270 = FACE_OUTER_BOUND ( 'NONE', #21052, .T. ) ;
#20271 = CARTESIAN_POINT ( 'NONE',  ( 8.732865712828660421, 190.3249964942741883, 274.4707185275763095 ) ) ;
#20272 = CARTESIAN_POINT ( 'NONE',  ( 163.9999999999998863, 18.00000000000000355, -8.000000000002268408 ) ) ;
#20273 = DIRECTION ( 'NONE',  ( -0.9999164797902015955, -4.476705744456278510E-15, 0.01292414190464144692 ) ) ;
#20274 = CONICAL_SURFACE ( 'NONE', #9275, 4.999999999999990230, 1.047197551196595855 ) ;
#20275 = CARTESIAN_POINT ( 'NONE',  ( -39.47524343981440609, 107.3883277703368861, 71.96416890068093153 ) ) ;
#20276 = FACE_OUTER_BOUND ( 'NONE', #20370, .T. ) ;
#20277 = DIRECTION ( 'NONE',  ( 0.9909299940865187173, -0.1338359446631173233, -0.01207007604876291287 ) ) ;
#20278 = ORIENTED_EDGE ( 'NONE', *, *, #8501, .F. ) ;
#20279 = EDGE_CURVE ( 'NONE', #2837, #10707, #1971, .T. ) ;
#20280 = DIRECTION ( 'NONE',  ( -0.9999164797902015955, -2.001050586450178695E-22, 0.01292414190464131335 ) ) ;
#20281 = ORIENTED_EDGE ( 'NONE', *, *, #21416, .T. ) ;
#20282 = CARTESIAN_POINT ( 'NONE',  ( -110.3526887502521561, 77.12912189496638860, -26.57600582461509475 ) ) ;
#20283 = CARTESIAN_POINT ( 'NONE',  ( -12.88085435000319912, 181.6037740665256877, 307.3265075889623290 ) ) ;
#20284 = ORIENTED_EDGE ( 'NONE', *, *, #7520, .T. ) ;
#20285 = VECTOR ( 'NONE', #8268, 999.9999999999998863 ) ;
#20286 = ORIENTED_EDGE ( 'NONE', *, *, #21950, .T. ) ;
#20287 = AXIS2_PLACEMENT_3D ( 'NONE', #10528, #2029, #9130 ) ;
#20288 = AXIS2_PLACEMENT_3D ( 'NONE', #11753, #13262, #16821 ) ;
#20289 = DIRECTION ( 'NONE',  ( -7.176269450075762180E-19, 1.000000000000000000, -5.550596000020001457E-17 ) ) ;
#20290 = EDGE_CURVE ( 'NONE', #14492, #5147, #10797, .T. ) ;
#20291 = EDGE_CURVE ( 'NONE', #7696, #9627, #8965, .T. ) ;
#20292 = DIRECTION ( 'NONE',  ( -0.9999164797902015955, -2.001050586450179636E-22, 0.01292414190464084844 ) ) ;
#20293 = EDGE_CURVE ( 'NONE', #12189, #850, #19864, .T. ) ;
#20294 = DIRECTION ( 'NONE',  ( 0.01111468050521610164, -0.5103046645782707280, 0.8599218645824314722 ) ) ;
#20295 = VECTOR ( 'NONE', #5140, 999.9999999999998863 ) ;
#20296 = CIRCLE ( 'NONE', #2710, 3.399999999999991918 ) ;
#20297 = EDGE_LOOP ( 'NONE', ( #17552, #13996 ) ) ;
#20298 = B_SPLINE_CURVE_WITH_KNOTS ( 'NONE', 3,
 ( #1354, #11685, #15374, #18799, #3062, #20628, #12133, #18903 ),
 .UNSPECIFIED., .F., .F.,
 ( 4, 2, 2, 4 ),
 ( 0.005257893453559938333, 0.006567392922673252059, 0.007876892391786564918, 0.01049589133001322533 ),
 .UNSPECIFIED. ) ;
#20299 = DIRECTION ( 'NONE',  ( 0.9934404589540163366, 0.1135548637187057258, -0.01346653032743021922 ) ) ;
#20300 = DIRECTION ( 'NONE',  ( -7.176269450075762180E-19, 1.000000000000000000, -5.550596000020001457E-17 ) ) ;
#20301 = ORIENTED_EDGE ( 'NONE', *, *, #6526, .F. ) ;
#20302 = CARTESIAN_POINT ( 'NONE',  ( -48.91844876508264406, 94.45452722259994971, 84.00069590936301722 ) ) ;
#20303 = DIRECTION ( 'NONE',  ( 0.3101392564284315978, 0.9506461370142478273, -0.009250070373107145000 ) ) ;
#20304 = CARTESIAN_POINT ( 'NONE',  ( -46.67642080778155389, 127.4153035195788846, 257.4621697307391059 ) ) ;
#20305 = AXIS2_PLACEMENT_3D ( 'NONE', #8515, #22063, #18748 ) ;
#20306 = ORIENTED_EDGE ( 'NONE', *, *, #14210, .F. ) ;
#20307 = EDGE_CURVE ( 'NONE', #559, #8361, #1994, .T. ) ;
#20308 = CARTESIAN_POINT ( 'NONE',  ( -154.0000000000000000, 18.00000000000000355, -53.76161406891256433 ) ) ;
#20309 = AXIS2_PLACEMENT_3D ( 'NONE', #6785, #20795, #12082 ) ;
#20310 = EDGE_CURVE ( 'NONE', #3219, #19439, #16241, .T. ) ;
#20311 = DIRECTION ( 'NONE',  ( -2.025474946048326158E-22, 1.000000000000000000, -1.876735158486679638E-22 ) ) ;
#20312 = ADVANCED_FACE ( 'NONE', ( #830 ), #9421, .T. ) ;
#20313 = LINE ( 'NONE', #4791, #17244 ) ;
#20314 = ORIENTED_EDGE ( 'NONE', *, *, #6929, .T. ) ;
#20315 = VECTOR ( 'NONE', #1985, 999.9999999999998863 ) ;
#20316 = UNCERTAINTY_MEASURE_WITH_UNIT (LENGTH_MEASURE( 1.000000000000000082E-05 ), #12330, 'distance_accuracy_value', 'NONE');
#20317 = CARTESIAN_POINT ( 'NONE',  ( 161.9999999999992610, 20.00000000000000000, -53.76161406891482386 ) ) ;
#20318 = DIRECTION ( 'NONE',  ( 0.9999164797902015955, 6.965998958219364448E-18, -0.01292414190464157182 ) ) ;
#20319 = SHAPE_DEFINITION_REPRESENTATION ( #12360, #938 ) ;
#20320 = ORIENTED_EDGE ( 'NONE', *, *, #18342, .F. ) ;
#20321 = VECTOR ( 'NONE', #8642, 1000.000000000000000 ) ;
#20322 = CARTESIAN_POINT ( 'NONE',  ( 3.898201936395599532, 166.6627968962365287, 301.5965304707955852 ) ) ;
#20323 = CARTESIAN_POINT ( 'NONE',  ( -50.99154849761720243, 113.0663986884224812, -43.53140896659793668 ) ) ;
#20324 = EDGE_CURVE ( 'NONE', #9955, #1394, #13810, .T. ) ;
#20325 = CARTESIAN_POINT ( 'NONE',  ( 38.46706438352715196, 91.17157287525388654, -85.27439087629288395 ) ) ;
#20326 = CARTESIAN_POINT ( 'NONE',  ( -14.11265002968298177, 325.6970952274145361, 313.9537617855303324 ) ) ;
#20327 = CARTESIAN_POINT ( 'NONE',  ( -10.85567112094788200, 105.6999953372425409, 127.2994028633183063 ) ) ;
#20328 = VERTEX_POINT ( 'NONE', #9668 ) ;
#20329 = CARTESIAN_POINT ( 'NONE',  ( -1.163172771417702700, 81.99999999999998579, -89.99248318111824574 ) ) ;
#20330 = DIRECTION ( 'NONE',  ( 0.9999164797902015955, 6.965998958219364448E-18, -0.01292414190464157182 ) ) ;
#20331 = LINE ( 'NONE', #6207, #18851 ) ;
#20332 = ORIENTED_EDGE ( 'NONE', *, *, #18050, .F. ) ;
#20333 = CARTESIAN_POINT ( 'NONE',  ( 36.07212464706828570, 94.02752048664899576, -83.44565016930062029 ) ) ;
#20334 = ORIENTED_EDGE ( 'NONE', *, *, #20661, .T. ) ;
#20335 = DIRECTION ( 'NONE',  ( -0.01292394549866731843, -0.005513023399720594006, -0.9999012842304693116 ) ) ;
#20336 = CARTESIAN_POINT ( 'NONE',  ( -14.37471740060550118, 109.6998846769365628, 127.3137863664913425 ) ) ;
#20337 = AXIS2_PLACEMENT_3D ( 'NONE', #18373, #6851, #22559 ) ;
#20338 = LINE ( 'NONE', #18945, #9445 ) ;
#20339 = CARTESIAN_POINT ( 'NONE',  ( -49.99582398951010731, 170.0000000000000284, 0.6462070952320568828 ) ) ;
#20340 = ADVANCED_FACE ( 'NONE', ( #12673 ), #5982, .T. ) ;
#20341 = EDGE_LOOP ( 'NONE', ( #4044, #13405, #18608, #1996, #10990 ) ) ;
#20342 = LINE ( 'NONE', #20553, #8514 ) ;
#20343 = CARTESIAN_POINT ( 'NONE',  ( 41.59208321381912299, 72.00000000000000000, 84.46951292587608862 ) ) ;
#20344 = ORIENTED_EDGE ( 'NONE', *, *, #21990, .T. ) ;
#20345 = VECTOR ( 'NONE', #13284, 1000.000000000000227 ) ;
#20346 = CARTESIAN_POINT ( 'NONE',  ( -162.0000000000000000, 2.000000000000000000, -53.76161406891256433 ) ) ;
#20347 = DIRECTION ( 'NONE',  ( 0.01292394549866733230, 0.005513023399720419666, 0.9999012842304692006 ) ) ;
#20348 = ORIENTED_EDGE ( 'NONE', *, *, #11607, .T. ) ;
#20349 = CARTESIAN_POINT ( 'NONE',  ( -66.75560256528235925, 192.1022009597331817, 19.34154534151025118 ) ) ;
#20350 = CARTESIAN_POINT ( 'NONE',  ( -88.16383505568140322, 88.29998048453171577, 52.88219642818270216 ) ) ;
#20351 = AXIS2_PLACEMENT_3D ( 'NONE', #7370, #16137, #375 ) ;
#20352 = ORIENTED_EDGE ( 'NONE', *, *, #8776, .T. ) ;
#20353 = EDGE_CURVE ( 'NONE', #1217, #1291, #9316, .T. ) ;
#20354 = CARTESIAN_POINT ( 'NONE',  ( -37.48841359254407735, 105.6219042656103255, 92.61087584162487474 ) ) ;
#20355 = DIRECTION ( 'NONE',  ( -1.362186893977296031E-14, 0.000000000000000000, 1.000000000000000000 ) ) ;
#20356 = FACE_OUTER_BOUND ( 'NONE', #9444, .T. ) ;
#20357 = FACE_OUTER_BOUND ( 'NONE', #21869, .T. ) ;
#20358 = LINE ( 'NONE', #21941, #2716 ) ;
#20359 = CYLINDRICAL_SURFACE ( 'NONE', #10779, 7.999999999999985789 ) ;
#20360 = EDGE_LOOP ( 'NONE', ( #22527, #5984, #17724, #21444 ) ) ;
#20361 = DIRECTION ( 'NONE',  ( -0.01292394549866695240, -0.005513023399725255208, -0.9999012842304693116 ) ) ;
#20362 = CARTESIAN_POINT ( 'NONE',  ( -88.74294073166163344, 70.70905333810220839, 62.85632276041776123 ) ) ;
#20363 = CARTESIAN_POINT ( 'NONE',  ( -64.98709011851474315, 170.4756630735863041, 1.418865331364558058 ) ) ;
#20364 = CARTESIAN_POINT ( 'NONE',  ( -40.51791796528902267, 94.71334217791753929, 83.69094846550264322 ) ) ;
#20365 = FACE_OUTER_BOUND ( 'NONE', #21852, .T. ) ;
#20366 = AXIS2_PLACEMENT_3D ( 'NONE', #11257, #6528, #18263 ) ;
#20367 = PRODUCT_DEFINITION_SHAPE ( 'NONE', 'NONE',  #22686 ) ;
#20368 = DIRECTION ( 'NONE',  ( 1.396592535537253658E-14, 0.000000000000000000, 1.000000000000000000 ) ) ;
#20369 = CARTESIAN_POINT ( 'NONE',  ( -11.09605440033590185, 186.4570468891244559, 320.9292597536728522 ) ) ;
#20370 = EDGE_LOOP ( 'NONE', ( #20348, #19713, #10579, #20209 ) ) ;
#20371 = CARTESIAN_POINT ( 'NONE',  ( -12.94603199877754918, 186.2120210550076536, 276.6147472438746604 ) ) ;
#20372 = ORIENTED_EDGE ( 'NONE', *, *, #19735, .F. ) ;
#20373 = ORIENTED_EDGE ( 'NONE', *, *, #14897, .T. ) ;
#20374 = CARTESIAN_POINT ( 'NONE',  ( 42.79028061014420103, 106.8061942917681364, 70.38622059413428644 ) ) ;
#20375 = VERTEX_POINT ( 'NONE', #4017 ) ;
#20376 = EDGE_CURVE ( 'NONE', #7407, #20796, #14117, .T. ) ;
#20377 = CARTESIAN_POINT ( 'NONE',  ( -49.15619943964080818, 107.7496120479954982, 70.42164486253489031 ) ) ;
#20378 = EDGE_CURVE ( 'NONE', #3397, #18358, #7501, .T. ) ;
#20379 = CARTESIAN_POINT ( 'NONE',  ( 105.9973908263408902, 79.15210294646411171, -29.40494008559776518 ) ) ;
#20380 = LINE ( 'NONE', #1673, #872 ) ;
#20381 = DIRECTION ( 'NONE',  ( 7.125109674141484573E-05, -0.9999848031710252272, 0.005512562950851785694 ) ) ;
#20382 = CARTESIAN_POINT ( 'NONE',  ( -90.43474204040838060, 77.12912189496637438, 31.17139488067998343 ) ) ;
#20383 = DIRECTION ( 'NONE',  ( 0.01292394549866738782, 0.005513023399720468239, 0.9999012842304692006 ) ) ;
#20384 = LINE ( 'NONE', #5924, #1628 ) ;
#20385 = FACE_OUTER_BOUND ( 'NONE', #14352, .T. ) ;
#20386 = ORIENTED_EDGE ( 'NONE', *, *, #3297, .F. ) ;
#20387 = PLANE ( 'NONE',  #1222 ) ;
#20388 = ORIENTED_EDGE ( 'NONE', *, *, #11529, .T. ) ;
#20389 = PRODUCT_DEFINITION ( 'UNKNOWN', '', #19444, #8563 ) ;
#20390 = ORIENTED_EDGE ( 'NONE', *, *, #18322, .F. ) ;
#20391 = DIRECTION ( 'NONE',  ( 0.9232306267972772984, 0.000000000000000000, -0.3842462878721232822 ) ) ;
#20392 = CARTESIAN_POINT ( 'NONE',  ( -8.664060416302492129, 185.3179921677720472, 305.1700144434819322 ) ) ;
#20393 = EDGE_LOOP ( 'NONE', ( #10469, #9381, #2694, #4880 ) ) ;
#20394 = CARTESIAN_POINT ( 'NONE',  ( -2.096375399687082197, 190.2200455327031534, 274.6112675210154634 ) ) ;
#20395 = VERTEX_POINT ( 'NONE', #22555 ) ;
#20396 = DIRECTION ( 'NONE',  ( 0.000000000000000000, 0.000000000000000000, 1.000000000000000000 ) ) ;
#20397 = EDGE_CURVE ( 'NONE', #8988, #13237, #2772, .T. ) ;
#20398 = CARTESIAN_POINT ( 'NONE',  ( -29.30063050186588214, 189.4444907833431273, -100.4463829504137209 ) ) ;
#20399 = CARTESIAN_POINT ( 'NONE',  ( -10.85624112972181621, 113.6998737626107641, 127.2553023597115214 ) ) ;
#20400 = DIRECTION ( 'NONE',  ( -0.4397038457472307593, 0.000000000000000000, 0.8981428216242088869 ) ) ;
#20401 = VERTEX_POINT ( 'NONE', #13984 ) ;
#20402 = CARTESIAN_POINT ( 'NONE',  ( -15.22406540918863982, 178.2721462461353497, 317.5143574882988560 ) ) ;
#20403 = VERTEX_POINT ( 'NONE', #5114 ) ;
#20404 = CARTESIAN_POINT ( 'NONE',  ( 109.5708359150300168, 75.34617192694389587, -10.75083194752833826 ) ) ;
#20405 = CARTESIAN_POINT ( 'NONE',  ( -13.92525281995234820, 325.7770340667113942, 328.4523304068723064 ) ) ;
#20406 = DIRECTION ( 'NONE',  ( -2.025474946048326158E-22, 1.000000000000000000, -1.876735158486679638E-22 ) ) ;
#20407 = EDGE_LOOP ( 'NONE', ( #18856, #16788, #10266, #18440 ) ) ;
#20408 = DIRECTION ( 'NONE',  ( -5.440186201345738641E-18, -1.000000000000000000, -1.334940939666364181E-17 ) ) ;
#20409 = EDGE_CURVE ( 'NONE', #13676, #11611, #20331, .T. ) ;
#20410 = CYLINDRICAL_SURFACE ( 'NONE', #16375, 75.00000000000002842 ) ;
#20411 = DIRECTION ( 'NONE',  ( 2.025474946048326158E-22, -1.000000000000000000, 1.876735158486679638E-22 ) ) ;
#20412 = CARTESIAN_POINT ( 'NONE',  ( -26.33924170010756427, 324.2792865754714171, 309.1008800470122537 ) ) ;
#20413 = ADVANCED_FACE ( 'NONE', ( #18509 ), #10309, .F. ) ;
#20414 = CARTESIAN_POINT ( 'NONE',  ( 51.40965114598606078, 154.9164872300239040, 274.0445329540610828 ) ) ;
#20415 = ORIENTED_EDGE ( 'NONE', *, *, #16308, .T. ) ;
#20416 = DIRECTION ( 'NONE',  ( 0.9999164797902017066, 2.001050586450178931E-22, -0.01292414190464131508 ) ) ;
#20417 = CONICAL_SURFACE ( 'NONE', #13486, 9.000000000000001776, 1.047197551196594301 ) ;
#20418 = LINE ( 'NONE', #11837, #84 ) ;
#20419 = CONTEXT_DEPENDENT_SHAPE_REPRESENTATION ( #4249, #12136 ) ;
#20420 = ADVANCED_FACE ( 'NONE', ( #10534 ), #17442, .F. ) ;
#20422 = EDGE_LOOP ( 'NONE', ( #7349, #16038, #3140, #2953 ) ) ;
#20421 = EDGE_LOOP ( 'NONE', ( #14, #4964, #20532, #6865 ) ) ;
#20423 = EDGE_CURVE ( 'NONE', #7668, #19030, #9881, .T. ) ;
#20424 = CARTESIAN_POINT ( 'NONE',  ( 90.77986998051285639, 77.66088650200015309, -32.02971036561883977 ) ) ;
#20425 = CARTESIAN_POINT ( 'NONE',  ( 13.66010556627975880, 189.9441383114576922, 320.7762228549422616 ) ) ;
#20426 = CARTESIAN_POINT ( 'NONE',  ( -20.57109388430227881, 136.7551719540686008, -44.05520973278501629 ) ) ;
#20427 = LINE ( 'NONE', #8160, #1933 ) ;
#20428 = EDGE_CURVE ( 'NONE', #4699, #18675, #13354, .T. ) ;
#20429 = CARTESIAN_POINT ( 'NONE',  ( 5.448539043597403264, 81.99999999999998579, -83.82247741134344210 ) ) ;
#20430 = CARTESIAN_POINT ( 'NONE',  ( 11.83347885643962982, 174.6861507205185546, 323.4518999165990181 ) ) ;
#20431 = DIRECTION ( 'NONE',  ( -2.025474946048326158E-22, 1.000000000000000000, -1.876735158486679638E-22 ) ) ;
#20432 = EDGE_LOOP ( 'NONE', ( #20475, #10076 ) ) ;
#20433 = DIRECTION ( 'NONE',  ( -2.025474946048326158E-22, 1.000000000000000000, -1.876735158486679638E-22 ) ) ;
#20434 = CARTESIAN_POINT ( 'NONE',  ( 39.99665919160806027, 170.0000000000000284, -0.5169656761856848970 ) ) ;
#20435 = ORIENTED_EDGE ( 'NONE', *, *, #7661, .T. ) ;
#20436 = DIRECTION ( 'NONE',  ( 0.01292394549866733230, 0.005513023399720419666, 0.9999012842304692006 ) ) ;
#20437 = DIRECTION ( 'NONE',  ( 0.9999164797902018176, 0.000000000000000000, -0.01292414190463827932 ) ) ;
#20438 = CARTESIAN_POINT ( 'NONE',  ( 51.99565694909048830, 170.0000000000000284, -0.6720553790413839046 ) ) ;
#20439 = CARTESIAN_POINT ( 'NONE',  ( -44.65269467507050649, 173.1465938866814724, 27.16116318951803521 ) ) ;
#20440 = VECTOR ( 'NONE', #17831, 1000.000000000000000 ) ;
#20441 = EDGE_CURVE ( 'NONE', #5676, #6995, #10062, .T. ) ;
#20442 = ORIENTED_EDGE ( 'NONE', *, *, #15024, .F. ) ;
#20443 = CARTESIAN_POINT ( 'NONE',  ( 63.79288799738544213, 189.4876967392748384, -93.81203076765316951 ) ) ;
#20444 = CARTESIAN_POINT ( 'NONE',  ( -51.18808688065827539, 114.3180568159422563, 170.6814081060424826 ) ) ;
#20445 = ORIENTED_EDGE ( 'NONE', *, *, #18247, .T. ) ;
#20446 = CARTESIAN_POINT ( 'NONE',  ( 47.71445816105992321, 95.00723670396115494, -44.72354054884888086 ) ) ;
#20447 = ADVANCED_FACE ( 'NONE', ( #21915 ), #15949, .F. ) ;
#20448 = CARTESIAN_POINT ( 'NONE',  ( -41.00000899811524846, 169.5540992312279229, 273.1580453575298293 ) ) ;
#20449 = VERTEX_POINT ( 'NONE', #3521 ) ;
#20450 = LINE ( 'NONE', #20230, #18659 ) ;
#20451 = CARTESIAN_POINT ( 'NONE',  ( -90.14583285889521846, 87.30743587841715225, 51.21137444554536700 ) ) ;
#20452 = ORIENTED_EDGE ( 'NONE', *, *, #11745, .T. ) ;
#20453 = ADVANCED_FACE ( 'NONE', ( #8672 ), #21065, .F. ) ;
#20454 = VECTOR ( 'NONE', #14833, 999.9999999999998863 ) ;
#20455 = EDGE_CURVE ( 'NONE', #20395, #17187, #20973, .T. ) ;
#20456 = CARTESIAN_POINT ( 'NONE',  ( -10.85975448567659463, 163.0086244145724379, 126.9834806368866111 ) ) ;
#20457 = DIRECTION ( 'NONE',  ( 2.025474946048326158E-22, -1.000000000000000000, 1.876735158486679638E-22 ) ) ;
#20458 = CARTESIAN_POINT ( 'NONE',  ( 1.143866695291850588, 165.4878681845327151, 88.49880848915942977 ) ) ;
#20459 = CYLINDRICAL_SURFACE ( 'NONE', #15885, 2.000000000000004885 ) ;
#20460 = CARTESIAN_POINT ( 'NONE',  ( -88.17341836116958120, 88.91892192788692739, 51.95902595935821466 ) ) ;
#20461 = CARTESIAN_POINT ( 'NONE',  ( -88.83250513209149801, 79.73807450349757175, 30.77911165157504314 ) ) ;
#20462 = DIRECTION ( 'NONE',  ( -0.01292394549866632963, -0.005513023399716958026, -0.9999012842304692006 ) ) ;
#20463 = B_SPLINE_CURVE_WITH_KNOTS ( 'NONE', 3,
 ( #14543, #20013, #10959, #18306 ),
 .UNSPECIFIED., .F., .F.,
 ( 4, 4 ),
 ( 0.000000000000000000, 0.0001183016465591462605 ),
 .UNSPECIFIED. ) ;
#20464 = VERTEX_POINT ( 'NONE', #12148 ) ;
#20465 = DIRECTION ( 'NONE',  ( 0.01292394549866737741, 0.005513023399721125699, 0.9999012842304693116 ) ) ;
#20466 = DIRECTION ( 'NONE',  ( -0.01292394549866632963, -0.005513023399716958026, -0.9999012842304692006 ) ) ;
#20467 = CARTESIAN_POINT ( 'NONE',  ( 88.55404276674168784, 79.97526064827546577, -31.48874835467967870 ) ) ;
#20468 = CARTESIAN_POINT ( 'NONE',  ( 14.14224087380716455, 105.6999953372425409, 126.9762993157022777 ) ) ;
#20469 = AXIS2_PLACEMENT_3D ( 'NONE', #8898, #7183, #14215 ) ;
#20470 = CARTESIAN_POINT ( 'NONE',  ( -12.30666638222278308, 148.2435203413120348, 278.7947897727548252 ) ) ;
#20471 = DIRECTION ( 'NONE',  ( 0.01292394549866743465, 0.005513023399721021615, 0.9999012842304692006 ) ) ;
#20472 = VECTOR ( 'NONE', #13173, 1000.000000000000000 ) ;
#20473 = EDGE_CURVE ( 'NONE', #9134, #10176, #6406, .T. ) ;
#20474 = CARTESIAN_POINT ( 'NONE',  ( -64.00269606583552218, 99.99497935025800643, 77.57957628177221920 ) ) ;
#20475 = ORIENTED_EDGE ( 'NONE', *, *, #2688, .F. ) ;
#20476 = CARTESIAN_POINT ( 'NONE',  ( -13.22220441251254286, 184.0858775641920886, 276.8515177789402060 ) ) ;
#20477 = EDGE_LOOP ( 'NONE', ( #12279, #2513 ) ) ;
#20478 = ORIENTED_EDGE ( 'NONE', *, *, #17994, .T. ) ;
#20479 = DIRECTION ( 'NONE',  ( 0.9999164797902017066, 2.001050586450178931E-22, -0.01292414190464131508 ) ) ;
#20480 = TOROIDAL_SURFACE ( 'NONE', #6558, 25.50000000000000355, 3.000000000000000000 ) ;
#20481 = B_SPLINE_CURVE_WITH_KNOTS ( 'NONE', 3,
 ( #7022, #3351, #19310, #3122, #17604, #1854, #22279, #13588 ),
 .UNSPECIFIED., .F., .F.,
 ( 4, 2, 2, 4 ),
 ( 0.000000000000000000, 0.001422162546572855154, 0.002133243819859289344, 0.002844325093145723751 ),
 .UNSPECIFIED. ) ;
#20482 = ORIENTED_EDGE ( 'NONE', *, *, #3762, .F. ) ;
#20483 = EDGE_CURVE ( 'NONE', #12094, #14118, #5230, .T. ) ;
#20484 = CARTESIAN_POINT ( 'NONE',  ( -50.07072918920412263, 106.9825899289013762, 71.40280719653912911 ) ) ;
#20485 = CARTESIAN_POINT ( 'NONE',  ( -86.05176612644825695, 104.9512348145193528, -68.52150138215246500 ) ) ;
#20486 = AXIS2_PLACEMENT_3D ( 'NONE', #6892, #1969, #10472 ) ;
#20487 = CARTESIAN_POINT ( 'NONE',  ( 85.71976348773939947, 75.03502047313104129, 1.478386053088734053 ) ) ;
#20488 = CARTESIAN_POINT ( 'NONE',  ( -92.60113547278139379, 70.26667278203282763, -59.37223626620097150 ) ) ;
#20489 = CYLINDRICAL_SURFACE ( 'NONE', #1467, 2.000000000000001332 ) ;
#20490 = CARTESIAN_POINT ( 'NONE',  ( 11.78110588053433716, 167.5436706889874756, 296.4892918070229939 ) ) ;
#20491 = CYLINDRICAL_SURFACE ( 'NONE', #9682, 4.500000000000006217 ) ;
#20492 = CARTESIAN_POINT ( 'NONE',  ( -51.91681395539769994, 189.5996271088964704, -72.01216872995293272 ) ) ;
#20493 = FACE_OUTER_BOUND ( 'NONE', #214, .T. ) ;
#20494 = CARTESIAN_POINT ( 'NONE',  ( 91.74710091628175235, 71.28171241778765932, 60.68341510339265454 ) ) ;
#20495 = ORIENTED_EDGE ( 'NONE', *, *, #19157, .T. ) ;
#20496 = VECTOR ( 'NONE', #14767, 1000.000000000000114 ) ;
#20497 = ORIENTED_EDGE ( 'NONE', *, *, #9480, .F. ) ;
#20498 = EDGE_CURVE ( 'NONE', #8236, #15668, #6448, .T. ) ;
#20499 = DIRECTION ( 'NONE',  ( 0.01111468050521496539, -0.5103046645782702839, 0.8599218645824316942 ) ) ;
#20500 = CARTESIAN_POINT ( 'NONE',  ( -13.47925116190214823, 109.7082975868306960, 128.8283231014776220 ) ) ;
#20501 = ADVANCED_FACE ( 'NONE', ( #11719 ), #13390, .T. ) ;
#20502 = CIRCLE ( 'NONE', #5084, 85.00000000000001421 ) ;
#20503 = EDGE_LOOP ( 'NONE', ( #17514, #15692, #13296, #12413 ) ) ;
#20504 = ORIENTED_EDGE ( 'NONE', *, *, #12315, .T. ) ;
#20505 = DIRECTION ( 'NONE',  ( -0.000000000000000000, -1.000000000000000000, -0.000000000000000000 ) ) ;
#20506 = VERTEX_POINT ( 'NONE', #8037 ) ;
#20507 = CARTESIAN_POINT ( 'NONE',  ( -44.28529243912001334, 178.1224293456637042, 277.1536612075450421 ) ) ;
#20508 = VECTOR ( 'NONE', #7359, 1000.000000000000114 ) ;
#20509 = ORIENTED_EDGE ( 'NONE', *, *, #138, .T. ) ;
#20510 = DIRECTION ( 'NONE',  ( -7.125109674025824596E-05, 0.9999848031710253382, -0.005512562950849464634 ) ) ;
#20511 = AXIS2_PLACEMENT_3D ( 'NONE', #18783, #4978, #20381 ) ;
#20512 = CARTESIAN_POINT ( 'NONE',  ( -9.812611130992889841, 187.6968966475756986, 321.1611080588128289 ) ) ;
#20513 = DIRECTION ( 'NONE',  ( 0.000000000000000000, 1.000000000000000000, -0.000000000000000000 ) ) ;
#20514 = VECTOR ( 'NONE', #19704, 1000.000000000000000 ) ;
#20515 = DIRECTION ( 'NONE',  ( -0.9726991065672923042, -0.2316562896908775648, 0.01384960395994898168 ) ) ;
#20516 = DIRECTION ( 'NONE',  ( 0.01292394549866738782, 0.005513023399720468239, 0.9999012842304692006 ) ) ;
#20517 = FACE_OUTER_BOUND ( 'NONE', #14708, .T. ) ;
#20519 = DIRECTION ( 'NONE',  ( -0.000000000000000000, -1.000000000000000000, -0.000000000000000000 ) ) ;
#20518 = CARTESIAN_POINT ( 'NONE',  ( -38.41810471662249427, 96.40874508186763592, 84.69213597070189792 ) ) ;
#20520 = ORIENTED_EDGE ( 'NONE', *, *, #9034, .T. ) ;
#20521 = DIRECTION ( 'NONE',  ( -2.025474946048326158E-22, 1.000000000000000000, -1.876735158486679638E-22 ) ) ;
#20522 = B_SPLINE_CURVE_WITH_KNOTS ( 'NONE', 3,
 ( #17798, #7303, #5584, #2138, #12615, #430, #16189, #7428, #16309, #14575, #4421, #21755, #9834, #9616 ),
 .UNSPECIFIED., .F., .F.,
 ( 4, 2, 2, 2, 2, 2, 4 ),
 ( 0.000000000000000000, 0.001026194940722985208, 0.001539292411084444961, 0.002052389881445904497, 0.003078584822168817930, 0.003591682292530273997, 0.004104779762891730931 ),
 .UNSPECIFIED. ) ;
#20523 = CARTESIAN_POINT ( 'NONE',  ( -14.02864438394168722, 325.7329298795136197, 320.4531201330285626 ) ) ;
#20524 = CARTESIAN_POINT ( 'NONE',  ( -12.33415390922155019, 182.0798801194594603, 322.4718643837915124 ) ) ;
#20525 = AXIS2_PLACEMENT_3D ( 'NONE', #17826, #7331, #575 ) ;
#20526 = VECTOR ( 'NONE', #5769, 1000.000000000000000 ) ;
#20527 = CARTESIAN_POINT ( 'NONE',  ( -27.31669362735653905, 324.2032591843751561, 317.9607093345767908 ) ) ;
#20528 = CARTESIAN_POINT ( 'NONE',  ( -41.44484243847307425, 166.0778875772120671, 275.1831587074827326 ) ) ;
#20529 = DIRECTION ( 'NONE',  ( 0.01292394549866695240, 0.005513023399704438526, 0.9999012842304693116 ) ) ;
#20530 = VECTOR ( 'NONE', #10318, 1000.000000000000114 ) ;
#20531 = APPLICATION_PROTOCOL_DEFINITION ( 'draft international standard', 'automotive_design', 1998, #20689 ) ;
#20533 = ORIENTED_EDGE ( 'NONE', *, *, #7532, .T. ) ;
#20532 = ORIENTED_EDGE ( 'NONE', *, *, #7445, .F. ) ;
#20534 = EDGE_CURVE ( 'NONE', #6487, #2857, #14848, .T. ) ;
#20535 = CARTESIAN_POINT ( 'NONE',  ( 58.87479767622038906, 143.5880916635284166, 105.9939182712553105 ) ) ;
#20536 = DIRECTION ( 'NONE',  ( -2.025474946048326158E-22, 1.000000000000000000, -1.876735158486679638E-22 ) ) ;
#20537 = CARTESIAN_POINT ( 'NONE',  ( 4.195452682864946325, 166.7895964344300808, 324.5942600080963985 ) ) ;
#20538 = CARTESIAN_POINT ( 'NONE',  ( 3.833582208905060185, 166.6352317792379267, 296.5970240496429255 ) ) ;
#20539 = CIRCLE ( 'NONE', #22358, 109.9999999999999858 ) ;
#20540 = CARTESIAN_POINT ( 'NONE',  ( 9.674709713264089326E-15, 37.00000000000000711, 78.99999999999998579 ) ) ;
#20541 = CARTESIAN_POINT ( 'NONE',  ( 58.90831880861169623, 126.6021325681202825, 108.5873850519959092 ) ) ;
#20542 = AXIS2_PLACEMENT_3D ( 'NONE', #5014, #19266, #15509 ) ;
#20543 =( REPRESENTATION_RELATIONSHIP ('NONE','NONE', #11808, #7092 ) REPRESENTATION_RELATIONSHIP_WITH_TRANSFORMATION ( #11023 )SHAPE_REPRESENTATION_RELATIONSHIP( ) );
#20544 = VERTEX_POINT ( 'NONE', #22031 ) ;
#20545 = CARTESIAN_POINT ( 'NONE',  ( 49.39733347012933251, 108.7803151467795004, -46.95028962098039216 ) ) ;
#20546 = ORIENTED_EDGE ( 'NONE', *, *, #3149, .F. ) ;
#20547 = VECTOR ( 'NONE', #112, 1000.000000000000000 ) ;
#20548 = CARTESIAN_POINT ( 'NONE',  ( 86.05176612644827117, 104.9512348145193528, 68.52150138215245079 ) ) ;
#20549 = DIRECTION ( 'NONE',  ( -0.01292394549866739996, -0.005513023399721131770, -0.9999012842304692006 ) ) ;
#20550 = FACE_OUTER_BOUND ( 'NONE', #8729, .T. ) ;
#20551 = EDGE_CURVE ( 'NONE', #13286, #12735, #6848, .T. ) ;
#20552 = VERTEX_POINT ( 'NONE', #7196 ) ;
#20553 = CARTESIAN_POINT ( 'NONE',  ( -3.606137745152995233, 157.2416648407696016, 299.7452723209433998 ) ) ;
#20554 = VECTOR ( 'NONE', #21646, 1000.000000000000227 ) ;
#20555 = EDGE_CURVE ( 'NONE', #22603, #726, #12278, .T. ) ;
#20556 = EDGE_LOOP ( 'NONE', ( #16686, #9619, #16524, #5328 ) ) ;
#20557 = CARTESIAN_POINT ( 'NONE',  ( -44.54898248114630377, 168.6907664596094776, 35.18517999664061335 ) ) ;
#20558 = EDGE_CURVE ( 'NONE', #14473, #5655, #3456, .T. ) ;
#20559 = DIRECTION ( 'NONE',  ( 0.9770372205688159228, -0.2127605332646582692, -0.01145535281434409414 ) ) ;
#20560 = ORIENTED_EDGE ( 'NONE', *, *, #7083, .T. ) ;
#20561 = CIRCLE ( 'NONE', #7744, 10.00000000000001599 ) ;
#20562 = ORIENTED_EDGE ( 'NONE', *, *, #21304, .T. ) ;
#20563 = LINE ( 'NONE', #17141, #21569 ) ;
#20564 = AXIS2_PLACEMENT_3D ( 'NONE', #3612, #21297, #10623 ) ;
#20565 = CARTESIAN_POINT ( 'NONE',  ( -90.15594448151276197, 87.25008185477516065, 51.24627459905987337 ) ) ;
#20566 = ORIENTED_EDGE ( 'NONE', *, *, #8299, .T. ) ;
#20567 = EDGE_CURVE ( 'NONE', #18985, #20796, #429, .T. ) ;
#20568 = CARTESIAN_POINT ( 'NONE',  ( -73.19071663825569374, 95.81335214582355775, 82.11661254133679222 ) ) ;
#20569 = PRESENTATION_LAYER_ASSIGNMENT (  '', '', ( #1526 ) ) ;
#20570 = ADVANCED_FACE ( 'NONE', ( #21201 ), #6019, .F. ) ;
#20571 = CARTESIAN_POINT ( 'NONE',  ( -162.0000000000000000, 0.000000000000000000, 53.76161406891260697 ) ) ;
#20572 = DIRECTION ( 'NONE',  ( 0.01292394549866728200, 0.005513023399720295634, 0.9999012842304692006 ) ) ;
#20573 = EDGE_LOOP ( 'NONE', ( #19512, #16654, #19158, #13280 ) ) ;
#20574 = FILL_AREA_STYLE ('',( #5173 ) ) ;
#20575 = CARTESIAN_POINT ( 'NONE',  ( -88.18033096311128816, 89.00450046955621985, 51.18519472437992590 ) ) ;
#20576 = CARTESIAN_POINT ( 'NONE',  ( -92.46788464407291031, 79.04398536104955042, 28.62013883513304080 ) ) ;
#20577 = CARTESIAN_POINT ( 'NONE',  ( -1.163172771417702700, 81.99999999999998579, -89.99248318111824574 ) ) ;
#20578 = VERTEX_POINT ( 'NONE', #21313 ) ;
#20579 = EDGE_CURVE ( 'NONE', #14056, #16531, #3960, .T. ) ;
#20580 = ORIENTED_EDGE ( 'NONE', *, *, #15408, .T. ) ;
#20581 = ORIENTED_EDGE ( 'NONE', *, *, #21192, .F. ) ;
#20582 = CARTESIAN_POINT ( 'NONE',  ( -45.15312007873931321, 180.5703843163154261, 257.1494065962392597 ) ) ;
#20583 = CARTESIAN_POINT ( 'NONE',  ( -71.61338682171090397, 92.58578643762702143, -83.49564556265197268 ) ) ;
#20584 = DIRECTION ( 'NONE',  ( 0.01246513159388064687, 0.2641402835564749529, 0.9644037178988124071 ) ) ;
#20585 = CARTESIAN_POINT ( 'NONE',  ( -40.43031930919660510, 94.59775782198136085, 83.80669187395014319 ) ) ;
#20586 = B_SPLINE_CURVE_WITH_KNOTS ( 'NONE', 3,
 ( #2677, #13134, #14641, #7944, #4263, #4151, #18086 ),
 .UNSPECIFIED., .F., .F.,
 ( 4, 3, 4 ),
 ( -5.913099621787071171E-08, -6.617444900424221399E-24, 3.076089232683742422E-05 ),
 .UNSPECIFIED. ) ;
#20587 = AXIS2_PLACEMENT_3D ( 'NONE', #21596, #16478, #498 ) ;
#20588 = DIRECTION ( 'NONE',  ( 0.9934404589540163366, 0.1135548637187052540, -0.01346653032742946982 ) ) ;
#20589 = DIRECTION ( 'NONE',  ( 0.000000000000000000, 0.000000000000000000, 1.000000000000000000 ) ) ;
#20590 =( GEOMETRIC_REPRESENTATION_CONTEXT ( 3 ) GLOBAL_UNCERTAINTY_ASSIGNED_CONTEXT ( ( #19100 ) ) GLOBAL_UNIT_ASSIGNED_CONTEXT ( ( #2464, #18109, #21841 ) ) REPRESENTATION_CONTEXT ( 'NONE', 'WORKASPACE' ) );
#20591 = VECTOR ( 'NONE', #1525, 999.9999999999998863 ) ;
#20592 = EDGE_CURVE ( 'NONE', #5676, #10577, #14573, .T. ) ;
#20593 = EDGE_CURVE ( 'NONE', #15824, #17834, #201, .T. ) ;
#20594 = AXIS2_PLACEMENT_3D ( 'NONE', #18097, #7385, #8995 ) ;
#20595 = CARTESIAN_POINT ( 'NONE',  ( -64.02925735614492453, 99.81835863910170303, 75.52457935425162816 ) ) ;
#20596 = VERTEX_POINT ( 'NONE', #15840 ) ;
#20597 = CARTESIAN_POINT ( 'NONE',  ( -7.132951983518865724, 188.3585648203603000, 276.8586589376985785 ) ) ;
#20598 = EDGE_LOOP ( 'NONE', ( #3994, #19411, #14293, #13376 ) ) ;
#20599 = CARTESIAN_POINT ( 'NONE',  ( -21.36186403949424673, 189.4186551486401413, -105.2356049757943310 ) ) ;
#20600 = AXIS2_PLACEMENT_3D ( 'NONE', #7760, #13174, #18320 ) ;
#20602 = ORIENTED_EDGE ( 'NONE', *, *, #9503, .F. ) ;
#20601 = ORIENTED_EDGE ( 'NONE', *, *, #561, .T. ) ;
#20603 = TOROIDAL_SURFACE ( 'NONE', #2995, 124.0000000000000000, 2.000000000000000000 ) ;
#20604 = FACE_OUTER_BOUND ( 'NONE', #5076, .T. ) ;
#20605 = CARTESIAN_POINT ( 'NONE',  ( -88.04920282358598627, 72.63494618757752619, 61.76065790490801533 ) ) ;
#20606 = AXIS2_PLACEMENT_3D ( 'NONE', #937, #11038, #6329 ) ;
#20607 = CARTESIAN_POINT ( 'NONE',  ( 83.86322835067295500, 75.13004950108779667, 3.890786405216685839 ) ) ;
#20608 = CARTESIAN_POINT ( 'NONE',  ( -93.38631075262969716, 70.00000000000000000, -58.13036983636536803 ) ) ;
#20609 = EDGE_CURVE ( 'NONE', #10751, #9038, #10983, .T. ) ;
#20610 = DIRECTION ( 'NONE',  ( -0.9999164797902015955, 0.000000000000000000, 0.01292414190464162733 ) ) ;
#20611 = CARTESIAN_POINT ( 'NONE',  ( -42.64951291394369548, 126.1473081376431367, 27.39440536439884255 ) ) ;
#20612 = CARTESIAN_POINT ( 'NONE',  ( -15.30033708903644296, 245.0148258455450616, 307.9133183403766907 ) ) ;
#20613 = CYLINDRICAL_SURFACE ( 'NONE', #5235, 112.5000000000000142 ) ;
#20614 = CARTESIAN_POINT ( 'NONE',  ( 9.914309459522627321, 174.9920644939733734, 324.4751176552225616 ) ) ;
#20615 = DIRECTION ( 'NONE',  ( -2.025474946048326158E-22, 1.000000000000000000, -1.876735158486679638E-22 ) ) ;
#20616 = VERTEX_POINT ( 'NONE', #7300 ) ;
#20617 = B_SPLINE_CURVE_WITH_KNOTS ( 'NONE', 3,
 ( #6899, #17381, #18741, #19076, #17257, #11979, #3121, #10369 ),
 .UNSPECIFIED., .F., .F.,
 ( 4, 2, 2, 4 ),
 ( 0.000000000000000000, 0.001196880956175902120, 0.002393761912351804241, 0.004787523824703608481 ),
 .UNSPECIFIED. ) ;
#20618 = CARTESIAN_POINT ( 'NONE',  ( -40.56069593696665976, 106.8539497625728103, 71.50607459554618117 ) ) ;
#20619 = ORIENTED_EDGE ( 'NONE', *, *, #21534, .F. ) ;
#20620 = AXIS2_PLACEMENT_3D ( 'NONE', #13555, #10109, #1714 ) ;
#20621 = CIRCLE ( 'NONE', #20975, 2.499999999999988010 ) ;
#20622 = CIRCLE ( 'NONE', #17718, 95.00000000000001421 ) ;
#20623 = EDGE_CURVE ( 'NONE', #5930, #7993, #7082, .T. ) ;
#20624 = ORIENTED_EDGE ( 'NONE', *, *, #7223, .T. ) ;
#20625 = CARTESIAN_POINT ( 'NONE',  ( 92.40872671617952960, 72.00000000000000000, -33.19707612406969588 ) ) ;
#20626 = DIRECTION ( 'NONE',  ( -0.000000000000000000, -1.000000000000000000, -0.000000000000000000 ) ) ;
#20627 = ORIENTED_EDGE ( 'NONE', *, *, #1671, .F. ) ;
#20628 = CARTESIAN_POINT ( 'NONE',  ( 8.108149183870599686, 70.35701968572533360, -87.30072018181319038 ) ) ;
#20629 = EDGE_LOOP ( 'NONE', ( #16855, #12263 ) ) ;
#20630 = AXIS2_PLACEMENT_3D ( 'NONE', #13788, #14016, #19047 ) ;
#20631 = CARTESIAN_POINT ( 'NONE',  ( 12.53841518797468346, 187.5782767441390035, 322.9588541052213486 ) ) ;
#20632 = AXIS2_PLACEMENT_3D ( 'NONE', #7564, #19711, #3652 ) ;
#20633 = AXIS2_PLACEMENT_3D ( 'NONE', #1300, #22485, #20676 ) ;
#20634 = CYLINDRICAL_SURFACE ( 'NONE', #3405, 3.399999999999986144 ) ;
#20635 = LINE ( 'NONE', #22658, #8014 ) ;
#20636 = CARTESIAN_POINT ( 'NONE',  ( 40.25303659951292445, 125.7553391191873544, -44.78072676432201860 ) ) ;
#20637 = ADVANCED_FACE ( 'NONE', ( #14113, #21092 ), #12613, .F. ) ;
#20638 = ORIENTED_EDGE ( 'NONE', *, *, #15872, .T. ) ;
#20639 = EDGE_CURVE ( 'NONE', #5010, #19042, #2136, .T. ) ;
#20640 = FACE_OUTER_BOUND ( 'NONE', #1248, .T. ) ;
#20641 = ORIENTED_EDGE ( 'NONE', *, *, #18428, .F. ) ;
#20642 = CARTESIAN_POINT ( 'NONE',  ( -46.67741832313596717, 141.4150907639732679, 257.3849938494272465 ) ) ;
#20643 = ORIENTED_EDGE ( 'NONE', *, *, #18154, .T. ) ;
#20644 = CARTESIAN_POINT ( 'NONE',  ( -45.98860230557422568, 168.0766615966952884, -76.19549020176363285 ) ) ;
#20645 = EDGE_LOOP ( 'NONE', ( #9218, #12665, #2355, #3859, #562, #12450 ) ) ;
#20646 = DIRECTION ( 'NONE',  ( 7.125109674160258889E-05, -0.9999848031710252272, 0.005512562950849897447 ) ) ;
#20647 = CARTESIAN_POINT ( 'NONE',  ( -54.95085304196765463, 138.9353748712228196, 170.4764683766270252 ) ) ;
#20648 = LINE ( 'NONE', #1149, #14308 ) ;
#20649 = DIRECTION ( 'NONE',  ( 7.125109674364536131E-05, -0.9999848031710253382, 0.005512562950849705760 ) ) ;
#20650 = VECTOR ( 'NONE', #1108, 999.9999999999998863 ) ;
#20651 = ORIENTED_EDGE ( 'NONE', *, *, #15974, .T. ) ;
#20652 = AXIS2_PLACEMENT_3D ( 'NONE', #17668, #3860, #420 ) ;
#20653 = CARTESIAN_POINT ( 'NONE',  ( -23.29666191406895237, 324.6732912418805768, 320.5140407611397677 ) ) ;
#20654 = CARTESIAN_POINT ( 'NONE',  ( -90.17340840076944630, 87.01269140061864960, 51.39028561451661403 ) ) ;
#20655 = APPLICATION_PROTOCOL_DEFINITION ( 'draft international standard', 'automotive_design', 1998, #22565 ) ;
#20656 = AXIS2_PLACEMENT_3D ( 'NONE', #19778, #20015, #11198 ) ;
#20657 = ORIENTED_EDGE ( 'NONE', *, *, #672, .T. ) ;
#20658 = EDGE_CURVE ( 'NONE', #1989, #2734, #5693, .T. ) ;
#20659 = LINE ( 'NONE', #11949, #14806 ) ;
#20660 = CARTESIAN_POINT ( 'NONE',  ( -5.380589158003702188, 174.4012695080579078, 324.6770650933424918 ) ) ;
#20661 = EDGE_CURVE ( 'NONE', #22201, #20105, #22547, .T. ) ;
#20662 = DIRECTION ( 'NONE',  ( -0.01292414190463830014, 0.000000000000000000, -0.9999164797902017066 ) ) ;
#20663 = DIRECTION ( 'NONE',  ( 0.01292394549866738782, 0.005513023399720468239, 0.9999012842304692006 ) ) ;
#20664 = CIRCLE ( 'NONE', #18486, 4.374999999999991118 ) ;
#20665 = CARTESIAN_POINT ( 'NONE',  ( 8.819665691964022614, 81.43869406011346257, -89.42914081817023941 ) ) ;
#20666 = AXIS2_PLACEMENT_3D ( 'NONE', #19340, #10396, #10613 ) ;
#20667 = FACE_OUTER_BOUND ( 'NONE', #1490, .T. ) ;
#20668 = ORIENTED_EDGE ( 'NONE', *, *, #21833, .T. ) ;
#20669 = CARTESIAN_POINT ( 'NONE',  ( 49.22891015931647019, 112.6462081887176367, -44.82446383698096071 ) ) ;
#20670 = ORIENTED_EDGE ( 'NONE', *, *, #20718, .T. ) ;
#20671 = DIRECTION ( 'NONE',  ( 2.025474946048326158E-22, -1.000000000000000000, 1.876735158486679638E-22 ) ) ;
#20672 = CARTESIAN_POINT ( 'NONE',  ( -85.15765475724558087, 77.82445350946629503, 69.65678843057233394 ) ) ;
#20673 = CARTESIAN_POINT ( 'NONE',  ( -46.67741832313596717, 141.4150907639732679, 257.3849938494272465 ) ) ;
#20674 = CARTESIAN_POINT ( 'NONE',  ( -41.71846863476348233, 170.1783921329469251, 257.1623099180083045 ) ) ;
#20675 = EDGE_LOOP ( 'NONE', ( #10682, #19821, #18183, #14297 ) ) ;
#20676 = DIRECTION ( 'NONE',  ( 0.01292394549866738782, 0.005513023399720700692, 0.9999012842304693116 ) ) ;
#20677 = CARTESIAN_POINT ( 'NONE',  ( -65.93268019054298179, 104.4142135623730780, -71.73965483371374319 ) ) ;
#20678 = VECTOR ( 'NONE', #17741, 1000.000000000000000 ) ;
#20679 = VECTOR ( 'NONE', #8273, 1000.000000000000000 ) ;
#20680 = VERTEX_POINT ( 'NONE', #2256 ) ;
#20681 = CARTESIAN_POINT ( 'NONE',  ( 49.40009966013455056, 96.21415597129798414, -46.73627471826173974 ) ) ;
#20682 = CARTESIAN_POINT ( 'NONE',  ( -0.9951589266573748205, 72.00000000000000000, -76.99356894384553129 ) ) ;
#20683 = ORIENTED_EDGE ( 'NONE', *, *, #72, .T. ) ;
#20684 = CIRCLE ( 'NONE', #2367, 2.000000000000001332 ) ;
#20685 = CIRCLE ( 'NONE', #18852, 20.50000000000000711 ) ;
#20686 = DIRECTION ( 'NONE',  ( 0.01096700916508646859, -0.5290868411612599242, 0.8484968115555724388 ) ) ;
#20687 = CARTESIAN_POINT ( 'NONE',  ( -90.10158855731272354, 87.47818988973786247, 51.10719583609721894 ) ) ;
#20688 = VERTEX_POINT ( 'NONE', #9136 ) ;
#20689 = APPLICATION_CONTEXT ( 'automotive_design' ) ;
#20690 = DIRECTION ( 'NONE',  ( 7.125109674364536131E-05, -0.9999848031710253382, 0.005512562950849705760 ) ) ;
#20691 = DIRECTION ( 'NONE',  ( 7.125109674161246868E-05, -0.9999848031710253382, 0.005512562950850155054 ) ) ;
#20692 = CARTESIAN_POINT ( 'NONE',  ( -26.49735288203455497, 89.79919665824762376, -78.55966460526794037 ) ) ;
#20693 = AXIS2_PLACEMENT_3D ( 'NONE', #10808, #12650, #11141 ) ;
#20694 = DIRECTION ( 'NONE',  ( -0.7944560844389294552, 0.000000000000000000, -0.6073216033519345247 ) ) ;
#20695 = EDGE_CURVE ( 'NONE', #19328, #20235, #20684, .T. ) ;
#20696 = DIRECTION ( 'NONE',  ( 0.9999164797902015955, 0.000000000000000000, -0.01292414190463754553 ) ) ;
#20697 = DIRECTION ( 'NONE',  ( -0.9915597537056654032, 0.0006440578489082665614, 0.1296489106033952843 ) ) ;
#20698 = ORIENTED_EDGE ( 'NONE', *, *, #8132, .F. ) ;
#20699 = ORIENTED_EDGE ( 'NONE', *, *, #2424, .F. ) ;
#20700 = CARTESIAN_POINT ( 'NONE',  ( -54.94728336202077656, 88.83613623235449097, 170.7526477804645140 ) ) ;
#20701 = DIRECTION ( 'NONE',  ( 0.9999164797902017066, 2.001050586450180576E-22, -0.01292414190464044946 ) ) ;
#20702 = DIRECTION ( 'NONE',  ( -0.01292394549866739996, -0.005513023399721564584, -0.9999012842304692006 ) ) ;
#20703 = AXIS2_PLACEMENT_3D ( 'NONE', #6050, #13080, #2603 ) ;
#20704 = CARTESIAN_POINT ( 'NONE',  ( -59.21150349786374534, 114.3969391141714169, 163.9271365849814117 ) ) ;
#20705 = AXIS2_PLACEMENT_3D ( 'NONE', #16293, #10547, #22461 ) ;
#20706 = CARTESIAN_POINT ( 'NONE',  ( -13.23388004031103193, 148.9771369504019844, 276.9130093688816032 ) ) ;
#20707 = ORIENTED_EDGE ( 'NONE', *, *, #12077, .T. ) ;
#20708 = DIRECTION ( 'NONE',  ( 1.000000000000000000, 0.000000000000000000, 0.000000000000000000 ) ) ;
#20709 = DIRECTION ( 'NONE',  ( -0.4910069343201003411, 0.004767316193522950878, 0.8711426192914036859 ) ) ;
#20710 = CARTESIAN_POINT ( 'NONE',  ( 90.13422078941499649, 99.92632882282073581, 63.05520142610588152 ) ) ;
#20711 = EDGE_CURVE ( 'NONE', #10601, #11676, #8576, .T. ) ;
#20712 =( BOUNDED_CURVE ( )  B_SPLINE_CURVE ( 3, ( #14540, #2454, #20010, #9449 ),
 .UNSPECIFIED., .F., .T. ) 
 B_SPLINE_CURVE_WITH_KNOTS ( ( 4, 4 ),
 ( 0.5456322604206232940, 1.570796326794899667 ),
 .UNSPECIFIED. ) 
 CURVE ( )  GEOMETRIC_REPRESENTATION_ITEM ( )  RATIONAL_B_SPLINE_CURVE ( ( 1.000000000000000000, 0.9143207399647593769, 0.9143207399647593769, 1.000000000000000000 ) ) 
 REPRESENTATION_ITEM ( '' )  );
#20713 = DIRECTION ( 'NONE',  ( 0.000000000000000000, 1.000000000000000000, -0.000000000000000000 ) ) ;
#20714 = EDGE_LOOP ( 'NONE', ( #14827, #1454, #21954, #11798 ) ) ;
#20715 =( GEOMETRIC_REPRESENTATION_CONTEXT ( 3 ) GLOBAL_UNCERTAINTY_ASSIGNED_CONTEXT ( ( #3489 ) ) GLOBAL_UNIT_ASSIGNED_CONTEXT ( ( #4259, #7602, #21709 ) ) REPRESENTATION_CONTEXT ( 'NONE', 'WORKASPACE' ) );
#20716 = VERTEX_POINT ( 'NONE', #9020 ) ;
#20717 = DIRECTION ( 'NONE',  ( -2.025474946048326158E-22, 1.000000000000000000, -1.876735158486679638E-22 ) ) ;
#20718 = EDGE_CURVE ( 'NONE', #22024, #16835, #19479, .T. ) ;
#20719 = VERTEX_POINT ( 'NONE', #16069 ) ;
#20720 = DIRECTION ( 'NONE',  ( -1.000000000000000000, 0.000000000000000000, 2.449293598294699019E-16 ) ) ;
#20721 = CARTESIAN_POINT ( 'NONE',  ( -86.44937305384743809, 104.7459436402722446, -68.01917747034278250 ) ) ;
#20722 = EDGE_CURVE ( 'NONE', #22035, #18467, #14683, .T. ) ;
#20723 = CARTESIAN_POINT ( 'NONE',  ( 85.94671339373330454, 75.02078408288856792, 0.9116371949491822724 ) ) ;
#20724 = CARTESIAN_POINT ( 'NONE',  ( -45.07718948873534970, 165.9786531560170033, 257.2288776738097908 ) ) ;
#20725 = EDGE_CURVE ( 'NONE', #13213, #8991, #6948, .T. ) ;
#20726 = EDGE_LOOP ( 'NONE', ( #20806, #3391, #19424, #8970, #13829, #17720, #2590, #3673 ) ) ;
#20727 = DIRECTION ( 'NONE',  ( -0.9999164797902017066, -2.001050586450177285E-22, 0.01292414190464223969 ) ) ;
#20728 = CARTESIAN_POINT ( 'NONE',  ( 163.9999999999998295, 19.17157287525381193, -8.000000000002268408 ) ) ;
#20729 = CONICAL_SURFACE ( 'NONE', #6445, 3.399999999999986144, 1.029744258676653201 ) ;
#20730 = CARTESIAN_POINT ( 'NONE',  ( 6.781388072971601844, 30.00000000000000711, -83.91926714759891581 ) ) ;
#20731 = CYLINDRICAL_SURFACE ( 'NONE', #15699, 7.499999999999992006 ) ;
#20732 = LINE ( 'NONE', #8548, #18868 ) ;
#20733 = EDGE_CURVE ( 'NONE', #19627, #13282, #21863, .T. ) ;
#20734 = CARTESIAN_POINT ( 'NONE',  ( 91.23603883849617091, 79.86121811340019860, 30.82342686631245243 ) ) ;
#20735 = EDGE_CURVE ( 'NONE', #13713, #2836, #21638, .T. ) ;
#20736 = PLANE ( 'NONE',  #17654 ) ;
#20737 = LINE ( 'NONE', #12131, #1875 ) ;
#20738 = ORIENTED_EDGE ( 'NONE', *, *, #10359, .F. ) ;
#20739 = CARTESIAN_POINT ( 'NONE',  ( -91.23603883849615670, 78.43035437438882695, -30.82342686631250572 ) ) ;
#20740 = EDGE_LOOP ( 'NONE', ( #19807, #21498, #337, #11771 ) ) ;
#20741 = EDGE_CURVE ( 'NONE', #15997, #8292, #11446, .T. ) ;
#20742 = AXIS2_PLACEMENT_3D ( 'NONE', #7701, #12547, #3807 ) ;
#20743 = CARTESIAN_POINT ( 'NONE',  ( -70.11017230969864045, 70.50928942481357353, -84.76194619987022350 ) ) ;
#20744 = PRODUCT_DEFINITION_CONTEXT ( 'detailed design', #8506, 'design' ) ;
#20745 = DIRECTION ( 'NONE',  ( 0.000000000000000000, -0.005512562964840580192, -0.9999848057093461140 ) ) ;
#20746 = EDGE_CURVE ( 'NONE', #7048, #13100, #5851, .T. ) ;
#20747 = ORIENTED_EDGE ( 'NONE', *, *, #2061, .F. ) ;
#20748 = CARTESIAN_POINT ( 'NONE',  ( 13.10093069687895095, 187.3512383165488302, 322.9178784991170232 ) ) ;
#20749 = DIRECTION ( 'NONE',  ( 0.9999164797902017066, 2.001050586450178931E-22, -0.01292414190464131508 ) ) ;
#20750 = ORIENTED_EDGE ( 'NONE', *, *, #2884, .T. ) ;
#20751 = SURFACE_SIDE_STYLE ('',( #1585 ) ) ;
#20752 = DIRECTION ( 'NONE',  ( -0.01292394549866727679, -0.005513023399720742325, -0.9999012842304692006 ) ) ;
#20753 = ORIENTED_EDGE ( 'NONE', *, *, #2863, .T. ) ;
#20754 = DIRECTION ( 'NONE',  ( -0.9999164797902017066, -2.001050586450180576E-22, 0.01292414190464039048 ) ) ;
#20755 = ORIENTED_EDGE ( 'NONE', *, *, #832, .F. ) ;
#20756 = CARTESIAN_POINT ( 'NONE',  ( -7.336909845677233477, 105.7000452102326591, 127.2629691083419203 ) ) ;
#20757 = CARTESIAN_POINT ( 'NONE',  ( -41.67747345744867715, 165.9786531560170033, 257.1849355913340673 ) ) ;
#20758 = CARTESIAN_POINT ( 'NONE',  ( 59.68375553853174154, 126.9329139721035489, 168.5814621058240732 ) ) ;
#20759 = EDGE_CURVE ( 'NONE', #5504, #10072, #20384, .T. ) ;
#20760 = CARTESIAN_POINT ( 'NONE',  ( 48.31072223536580879, 166.8507685304811048, 256.0170097695140043 ) ) ;
#20761 = CARTESIAN_POINT ( 'NONE',  ( 23.31388521830841754, 181.4144828908144405, 256.2598013980683049 ) ) ;
#20762 = FACE_OUTER_BOUND ( 'NONE', #20503, .T. ) ;
#20763 = DIRECTION ( 'NONE',  ( 0.9999164797902015955, 6.965998958219364448E-18, -0.01292414190464157182 ) ) ;
#20764 = ITEM_DEFINED_TRANSFORMATION ( 'NONE', 'NONE', #386,  #6292 ) ;
#20766 = ORIENTED_EDGE ( 'NONE', *, *, #9630, .T. ) ;
#20765 = ORIENTED_EDGE ( 'NONE', *, *, #15808, .T. ) ;
#20767 = DIRECTION ( 'NONE',  ( 7.125109674160258889E-05, -0.9999848031710252272, 0.005512562950849897447 ) ) ;
#20768 = ADVANCED_FACE ( 'NONE', ( #4302 ), #771, .T. ) ;
#20769 = DIRECTION ( 'NONE',  ( 0.8981428216242086648, 0.000000000000000000, -0.4397038457472310924 ) ) ;
#20770 = CARTESIAN_POINT ( 'NONE',  ( -21.32529163372091219, 169.4339520569534159, -102.4060669292324661 ) ) ;
#20771 = LINE ( 'NONE', #1389, #16274 ) ;
#20772 = CIRCLE ( 'NONE', #11645, 2.000000000000001776 ) ;
#20773 = VERTEX_POINT ( 'NONE', #11674 ) ;
#20774 = ORIENTED_EDGE ( 'NONE', *, *, #6468, .F. ) ;
#20775 = CARTESIAN_POINT ( 'NONE',  ( 0.000000000000000000, 20.00000000000000000, 0.000000000000000000 ) ) ;
#20776 = DIRECTION ( 'NONE',  ( 5.440186201345738641E-18, 1.000000000000000000, 1.334940939666364181E-17 ) ) ;
#20777 = ORIENTED_EDGE ( 'NONE', *, *, #12257, .F. ) ;
#20778 = CARTESIAN_POINT ( 'NONE',  ( 50.35954681524507492, 109.7098288542535016, -44.82288763992134761 ) ) ;
#20779 = ORIENTED_EDGE ( 'NONE', *, *, #20759, .T. ) ;
#20780 =( NAMED_UNIT ( * ) SI_UNIT ( $, .STERADIAN. ) SOLID_ANGLE_UNIT ( ) );
#20781 = CARTESIAN_POINT ( 'NONE',  ( -92.40872671617950118, 72.00000000000000000, 33.19707612406966746 ) ) ;
#20782 = DIRECTION ( 'NONE',  ( 0.000000000000000000, 1.000000000000000000, 0.000000000000000000 ) ) ;
#20783 = DIRECTION ( 'NONE',  ( 0.6080604969667604554, 0.004419696743559108250, 0.7938783901261144971 ) ) ;
#20784 = EDGE_LOOP ( 'NONE', ( #1412, #3746, #2277 ) ) ;
#20785 = CARTESIAN_POINT ( 'NONE',  ( -4.762299381711034840, 326.7918550596768910, 320.2627991765112938 ) ) ;
#20786 = CYLINDRICAL_SURFACE ( 'NONE', #5323, 9.999999999999992895 ) ;
#20787 = VERTEX_POINT ( 'NONE', #9375 ) ;
#20788 = CARTESIAN_POINT ( 'NONE',  ( 48.12222853284146140, 95.06897948779807450, -44.83367642559105803 ) ) ;
#20789 = EDGE_CURVE ( 'NONE', #1532, #1991, #19951, .T. ) ;
#20790 = EDGE_CURVE ( 'NONE', #12915, #19373, #18567, .T. ) ;
#20791 = ORIENTED_EDGE ( 'NONE', *, *, #2780, .F. ) ;
#20792 = CARTESIAN_POINT ( 'NONE',  ( 91.64606417454449172, 70.03008549560414053, -60.83696323298806163 ) ) ;
#20793 = B_SPLINE_CURVE_WITH_KNOTS ( 'NONE', 3,
 ( #2713, #21744, #9726, #18121, #14674, #2371, #9364, #14913, #11217, #20139, #6039, #16401, #4409, #20035, #7630, #14561, #20267, #18224, #9247, #5916, #21519, #12953, #989, #11437, #2476, #7974, #9471, #16507, #6265, #760, #7759, #18448, #15012, #21964, #15468, #6713, #16843, #1105 ),
 .UNSPECIFIED., .F., .F.,
 ( 4, 2, 2, 2, 2, 2, 2, 2, 2, 2, 2, 2, 2, 2, 2, 2, 2, 2, 4 ),
 ( 0.01594779277582532295, 0.01694430233486374573, 0.01794081189390216852, 0.01893732145294058783, 0.01993383101197901061, 0.02093034057101743339, 0.02192685013005585271, 0.02292335968909427549, 0.02391986924813269827, 0.02491637880717111758, 0.02541463358669033418, 0.02591288836620954730, 0.02690939792524796315, 0.02790590748428638246, 0.02890241704332479483, 0.02940067182284402530, 0.02989892660236324884, 0.03089543616140169591, 0.03189194572044014991 ),
 .UNSPECIFIED. ) ;
#20794 = CARTESIAN_POINT ( 'NONE',  ( -90.14238824705606135, 87.32442042776537505, 51.20102670897820474 ) ) ;
#20795 = DIRECTION ( 'NONE',  ( 0.01292394549866742078, 0.005513023399720777019, 0.9999012842304693116 ) ) ;
#20797 = ORIENTED_EDGE ( 'NONE', *, *, #5993, .T. ) ;
#20796 = VERTEX_POINT ( 'NONE', #18330 ) ;
#20798 = ORIENTED_EDGE ( 'NONE', *, *, #10185, .T. ) ;
#20799 = CARTESIAN_POINT ( 'NONE',  ( -13.99926948760909795, 325.7454604562529425, 322.7258004511344325 ) ) ;
#20800 = LINE ( 'NONE', #8620, #16972 ) ;
#20801 = CARTESIAN_POINT ( 'NONE',  ( -22.15772835622063042, 88.61525343264318622, -77.39142602527519443 ) ) ;
#20802 = DIRECTION ( 'NONE',  ( -0.01292394549866738608, -0.005513023399720468239, -0.9999012842304692006 ) ) ;
#20803 = PRODUCT_DEFINITION ( 'UNKNOWN', '', #1856, #3271 ) ;
#20804 = CARTESIAN_POINT ( 'NONE',  ( -71.00742074342183230, 91.74173777283634479, -84.01159762260417097 ) ) ;
#20805 = ORIENTED_EDGE ( 'NONE', *, *, #1901, .F. ) ;
#20806 = ORIENTED_EDGE ( 'NONE', *, *, #5425, .F. ) ;
#20807 = ORIENTED_EDGE ( 'NONE', *, *, #5396, .F. ) ;
#20808 = CARTESIAN_POINT ( 'NONE',  ( -10.43849514614221974, 186.3215578479907037, 278.0845509935722930 ) ) ;
#20809 = DIRECTION ( 'NONE',  ( 0.000000000000000000, 0.000000000000000000, 1.000000000000000000 ) ) ;
#20810 = LINE ( 'NONE', #18867, #3559 ) ;
#20811 = FACE_OUTER_BOUND ( 'NONE', #17397, .T. ) ;
#20812 = CARTESIAN_POINT ( 'NONE',  ( -3.901390060011853400, 143.2576375794741068, 275.3477745180629768 ) ) ;
#20813 = CARTESIAN_POINT ( 'NONE',  ( 0.000000000000000000, 0.000000000000000000, 0.000000000000000000 ) ) ;
#20814 = CARTESIAN_POINT ( 'NONE',  ( -89.23620587891574019, 78.43035437438885538, -30.84927515012178389 ) ) ;
#20815 = FACE_OUTER_BOUND ( 'NONE', #527, .T. ) ;
#20816 = ADVANCED_FACE ( 'NONE', ( #4199 ), #11225, .T. ) ;
#20817 = LINE ( 'NONE', #17066, #10334 ) ;
#20818 = ORIENTED_EDGE ( 'NONE', *, *, #7649, .T. ) ;
#20819 = ORIENTED_EDGE ( 'NONE', *, *, #6433, .T. ) ;
#20820 = DIRECTION ( 'NONE',  ( 0.9999164797902017066, 6.965998958219365988E-18, -0.01292414190464157356 ) ) ;
#20821 = ORIENTED_EDGE ( 'NONE', *, *, #18267, .T. ) ;
#20822 = SURFACE_SIDE_STYLE ('',( #11780 ) ) ;
#20823 = FACE_OUTER_BOUND ( 'NONE', #8288, .T. ) ;
#20824 = CIRCLE ( 'NONE', #11306, 2.000000000000001776 ) ;
#20825 = DIRECTION ( 'NONE',  ( 0.01292414190465215537, 0.000000000000000000, 0.9999164797902015955 ) ) ;
#20826 = EDGE_CURVE ( 'NONE', #21984, #16088, #13034, .T. ) ;
#20827 = CYLINDRICAL_SURFACE ( 'NONE', #21016, 2.000000000000001776 ) ;
#20828 = CARTESIAN_POINT ( 'NONE',  ( 13.04685173701508205, 190.3009448115034843, 320.8498781618246198 ) ) ;
#20829 = CARTESIAN_POINT ( 'NONE',  ( 9.842922453853201858, 175.8895142040481403, 299.4686240604829663 ) ) ;
#20830 = CARTESIAN_POINT ( 'NONE',  ( 12.84822208535021915, 190.4846235402699790, 307.8504815015369900 ) ) ;
#20831 = LINE ( 'NONE', #5089, #11921 ) ;
#20832 = AXIS2_PLACEMENT_3D ( 'NONE', #15353, #10161, #20720 ) ;
#20833 = LINE ( 'NONE', #20734, #8080 ) ;
#20834 = ORIENTED_EDGE ( 'NONE', *, *, #1400, .T. ) ;
#20835 =( BOUNDED_CURVE ( )  B_SPLINE_CURVE ( 3, ( #17788, #9605, #4075, #5791 ),
 .UNSPECIFIED., .F., .T. ) 
 B_SPLINE_CURVE_WITH_KNOTS ( ( 4, 4 ),
 ( 4.712388980384689674, 6.283185307179586232 ),
 .UNSPECIFIED. ) 
 CURVE ( )  GEOMETRIC_REPRESENTATION_ITEM ( )  RATIONAL_B_SPLINE_CURVE ( ( 1.000000000000000000, 0.8047378541243649375, 0.8047378541243649375, 1.000000000000000000 ) ) 
 REPRESENTATION_ITEM ( '' )  );
#20836 = DIRECTION ( 'NONE',  ( -0.01292414190463832269, 0.000000000000000000, -0.9999164797902017066 ) ) ;
#20837 = CARTESIAN_POINT ( 'NONE',  ( 48.49599547156344670, 174.4605628858501802, 275.9746324660413279 ) ) ;
#20838 = VERTEX_POINT ( 'NONE', #9615 ) ;
#20839 = CYLINDRICAL_SURFACE ( 'NONE', #18992, 126.0000000000000000 ) ;
#20840 = AXIS2_PLACEMENT_3D ( 'NONE', #19911, #756, #5780 ) ;
#20841 = EDGE_CURVE ( 'NONE', #11917, #2955, #20147, .T. ) ;
#20842 = ORIENTED_EDGE ( 'NONE', *, *, #10996, .T. ) ;
#20843 = ADVANCED_FACE ( 'NONE', ( #4419 ), #18459, .F. ) ;
#20844 = CONICAL_SURFACE ( 'NONE', #21928, 3.309500000000002107, 0.7853981633974710386 ) ;
#20845 = AXIS2_PLACEMENT_3D ( 'NONE', #11525, #9795, #10134 ) ;
#20846 = PLANE ( 'NONE',  #3013 ) ;
#20847 = ORIENTED_EDGE ( 'NONE', *, *, #19074, .F. ) ;
#20848 = PLANE ( 'NONE',  #14837 ) ;
#20849 = CARTESIAN_POINT ( 'NONE',  ( -104.9011368644396640, 70.01236949047485325, 33.10239539927072627 ) ) ;
#20850 = EDGE_CURVE ( 'NONE', #20688, #11842, #13015, .T. ) ;
#20851 = DIRECTION ( 'NONE',  ( 7.125109674160258889E-05, -0.9999848031710252272, 0.005512562950849897447 ) ) ;
#20852 = ORIENTED_EDGE ( 'NONE', *, *, #8341, .T. ) ;
#20853 = ADVANCED_FACE ( 'NONE', ( #17420 ), #10080, .T. ) ;
#20854 = FACE_OUTER_BOUND ( 'NONE', #3980, .T. ) ;
#20855 = VERTEX_POINT ( 'NONE', #4870 ) ;
#20856 = DIRECTION ( 'NONE',  ( 0.9999164797902015955, 6.965998958219364448E-18, -0.01292414190464157182 ) ) ;
#20857 = AXIS2_PLACEMENT_3D ( 'NONE', #7051, #3934, #12357 ) ;
#20858 = EDGE_CURVE ( 'NONE', #19234, #11064, #8430, .T. ) ;
#20859 = CARTESIAN_POINT ( 'NONE',  ( -17.13003694822599954, 316.2264685093712160, 320.5456208367596105 ) ) ;
#20860 = CARTESIAN_POINT ( 'NONE',  ( -8.523216527044569446, 185.4125284852929099, 305.1540476800932424 ) ) ;
#20861 = AXIS2_PLACEMENT_3D ( 'NONE', #22569, #3430, #4912 ) ;
#20862 = DIRECTION ( 'NONE',  ( -0.9999164797902017066, -2.001050586450178931E-22, 0.01292414190464131508 ) ) ;
#20863 = VERTEX_POINT ( 'NONE', #6724 ) ;
#20864 = LINE ( 'NONE', #3419, #4077 ) ;
#20865 = B_SPLINE_CURVE_WITH_KNOTS ( 'NONE', 3,
 ( #21106, #15973, #3641, #12163, #21214, #17566, #10438, #1594, #8683, #6751, #10658, #5015, #19148, #20989, #101, #12288, #15510, #7096, #1937, #5243, #7210, #10782, #8929, #15622, #17337, #15734, #5470, #3425, #213, #17812, #14126, #17457, #1708, #14724, #22566, #12044, #12507, #3296, #6976, #19268, #14239, #6857, #8804, #8583, #5359, #10322 ),
 .UNSPECIFIED., .F., .F.,
 ( 4, 2, 2, 2, 2, 2, 2, 2, 2, 2, 2, 2, 2, 2, 2, 2, 2, 2, 2, 2, 2, 2, 4 ),
 ( 0.000000000000000000, 0.0007988346004489777592, 0.001597669200897955518, 0.003195338401795909736, 0.003994173002244886736, 0.004793007602693864604, 0.006390676803591825543, 0.007988346004489785615, 0.009586015205387746554, 0.01118368440628570923, 0.01278135360718367017, 0.01358018820763266105, 0.01437902280808165539, 0.01517785740853064627, 0.01597669200897963715, 0.01757436120987761544, 0.01917203041077558678, 0.01997086501122459154, 0.02076969961167359630, 0.02236736881257176540, 0.02396503801346993451, 0.02476387261391905376, 0.02556270721436816953 ),
 .UNSPECIFIED. ) ;
#20866 = CARTESIAN_POINT ( 'NONE',  ( 87.01081826484191595, 101.8285212125953763, -67.31825406265291178 ) ) ;
#20867 = CARTESIAN_POINT ( 'NONE',  ( -71.61338682171090397, 92.58578643762702143, -83.49564556265197268 ) ) ;
#20868 = DIRECTION ( 'NONE',  ( 0.01292394549866739996, 0.005513023399720822122, 0.9999012842304692006 ) ) ;
#20869 = ADVANCED_FACE ( 'NONE', ( #18786 ), #1345, .T. ) ;
#20870 = CARTESIAN_POINT ( 'NONE',  ( 38.46706438352715196, 91.17157287525388654, -85.27439087629288395 ) ) ;
#20871 = ORIENTED_EDGE ( 'NONE', *, *, #19929, .T. ) ;
#20872 = AXIS2_PLACEMENT_3D ( 'NONE', #16848, #18781, #1232 ) ;
#20873 = EDGE_CURVE ( 'NONE', #21242, #15318, #3090, .T. ) ;
#20874 = DIRECTION ( 'NONE',  ( -0.01292414190464115722, 0.000000000000000000, -0.9999164797902015955 ) ) ;
#20875 = AXIS2_PLACEMENT_3D ( 'NONE', #1314, #6794, #4948 ) ;
#20876 = LINE ( 'NONE', #1067, #18501 ) ;
#20877 = VECTOR ( 'NONE', #13668, 1000.000000000000227 ) ;
#20879 = VERTEX_POINT ( 'NONE', #1679 ) ;
#20878 = ORIENTED_EDGE ( 'NONE', *, *, #11291, .F. ) ;
#20880 = B_SPLINE_CURVE_WITH_KNOTS ( 'NONE', 3,
 ( #17359, #5035, #3446, #19172, #1726, #5491, #5151, #1955, #17587, #10457, #12190, #232, #10229, #22589, #12071, #19054 ),
 .UNSPECIFIED., .F., .F.,
 ( 4, 2, 2, 2, 2, 2, 2, 4 ),
 ( 1.040834085586084257E-17, 0.0004729024035692759587, 0.0009458048071385415090, 0.001891609614277086054, 0.002364512017846342063, 0.002837414421415598072, 0.003310316824984853648, 0.003783219228554109657 ),
 .UNSPECIFIED. ) ;
#20881 = LINE ( 'NONE', #15742, #19523 ) ;
#20882 = CARTESIAN_POINT ( 'NONE',  ( 58.06826235119833512, 126.2437860471384568, 43.59380157701544789 ) ) ;
#20883 = CARTESIAN_POINT ( 'NONE',  ( -41.47069032946998846, 166.0668615304125808, 273.1833561390217824 ) ) ;
#20884 = DIRECTION ( 'NONE',  ( 0.01035358732338034077, 0.000000000000000000, 0.9999464001782980560 ) ) ;
#20885 = EDGE_LOOP ( 'NONE', ( #3081, #19355, #15917, #4184 ) ) ;
#20886 = ORIENTED_EDGE ( 'NONE', *, *, #20293, .T. ) ;
#20887 = DIRECTION ( 'NONE',  ( -0.01292394549866731843, -0.005513023399720594006, -0.9999012842304693116 ) ) ;
#20888 = CARTESIAN_POINT ( 'NONE',  ( -56.11559749965279309, 143.5880916635282176, 107.4801945902891021 ) ) ;
#20889 = ORIENTED_EDGE ( 'NONE', *, *, #9478, .T. ) ;
#20890 = ADVANCED_FACE ( 'NONE', ( #8228 ), #17301, .F. ) ;
#20891 = CARTESIAN_POINT ( 'NONE',  ( 51.23232595389467292, 111.9218655262938995, -48.12066054576542484 ) ) ;
#20892 = VERTEX_POINT ( 'NONE', #20951 ) ;
#20893 = CARTESIAN_POINT ( 'NONE',  ( 44.03004128744986190, 171.4878726268958360, -75.33468125154308836 ) ) ;
#20894 = CARTESIAN_POINT ( 'NONE',  ( -1.163172771417702700, 69.99999999999998579, -89.99248318111824574 ) ) ;
#20895 = LINE ( 'NONE', #9048, #11074 ) ;
#20896 = CIRCLE ( 'NONE', #4751, 2.000000000000001776 ) ;
#20897 = AXIS2_PLACEMENT_3D ( 'NONE', #6365, #8200, #18972 ) ;
#20898 = ORIENTED_EDGE ( 'NONE', *, *, #9098, .T. ) ;
#20899 = SURFACE_SIDE_STYLE ('',( #3557 ) ) ;
#20900 = EDGE_LOOP ( 'NONE', ( #22198, #8006, #16376, #20445 ) ) ;
#20901 = CARTESIAN_POINT ( 'NONE',  ( 21.69134381229430275, 168.7570390772204405, 316.3235220979586870 ) ) ;
#20902 = EDGE_CURVE ( 'NONE', #7368, #17515, #1561, .T. ) ;
#20903 = AXIS2_PLACEMENT_3D ( 'NONE', #11470, #20173, #7791 ) ;
#20904 = CARTESIAN_POINT ( 'NONE',  ( 10.97572204090303138, 189.7859119041212637, 274.8914519908082070 ) ) ;
#20905 = ORIENTED_EDGE ( 'NONE', *, *, #19607, .F. ) ;
#20906 = CARTESIAN_POINT ( 'NONE',  ( -44.54898248114584192, 168.6907664596095913, 35.18517999664060625 ) ) ;
#20907 = CARTESIAN_POINT ( 'NONE',  ( -88.16945660481133018, 88.73583354750662977, 52.36250520916426865 ) ) ;
#20908 = CARTESIAN_POINT ( 'NONE',  ( -19.03062446302745414, 99.74539563421257071, 75.12800353666800390 ) ) ;
#20909 = VERTEX_POINT ( 'NONE', #22210 ) ;
#20910 = ORIENTED_EDGE ( 'NONE', *, *, #6838, .T. ) ;
#20911 = LINE ( 'NONE', #8293, #1521 ) ;
#20912 = CYLINDRICAL_SURFACE ( 'NONE', #10721, 2.000000000000001332 ) ;
#20913 = CARTESIAN_POINT ( 'NONE',  ( -0.9693106428480923187, 86.14745084375785211, -74.99373598426512899 ) ) ;
#20914 = PRODUCT_DEFINITION_FORMATION_WITH_SPECIFIED_SOURCE ( 'ANY', '', #15071, .NOT_KNOWN. ) ;
#20915 = CARTESIAN_POINT ( 'NONE',  ( 4.195452682864886818, 166.7895964344300239, 324.5942600080955458 ) ) ;
#20916 = CARTESIAN_POINT ( 'NONE',  ( 83.31510742684905324, 75.07738311394993502, -4.918051378794431550 ) ) ;
#20917 = FACE_OUTER_BOUND ( 'NONE', #15915, .T. ) ;
#20918 = ORIENTED_EDGE ( 'NONE', *, *, #8242, .T. ) ;
#20919 = EDGE_CURVE ( 'NONE', #12549, #19209, #21712, .T. ) ;
#20920 = AXIS2_PLACEMENT_3D ( 'NONE', #10749, #2232, #9006 ) ;
#20921 = ORIENTED_EDGE ( 'NONE', *, *, #10128, .F. ) ;
#20922 = ADVANCED_FACE ( 'NONE', ( #10169 ), #1452, .F. ) ;
#20923 = EDGE_LOOP ( 'NONE', ( #22156, #19515, #14072, #22217, #21542 ) ) ;
#20924 = DIRECTION ( 'NONE',  ( -0.01292394549866637994, -0.005513023399719273882, -0.9999012842304692006 ) ) ;
#20925 = CARTESIAN_POINT ( 'NONE',  ( -66.54547063575685684, 145.1911235850905371, 35.59905634788768225 ) ) ;
#20926 = CARTESIAN_POINT ( 'NONE',  ( -79.92740525950245001, 75.13699351169597662, 6.133505399301365735 ) ) ;
#20927 = CARTESIAN_POINT ( 'NONE',  ( -25.55593907343507709, 324.4110961426445101, 319.5660351319885990 ) ) ;
#20928 = DIRECTION ( 'NONE',  ( 7.125109674161259066E-05, -0.9999848031710252272, 0.005512562950850163727 ) ) ;
#20929 = FILL_AREA_STYLE_COLOUR ( '', #19966 ) ;
#20930 = VECTOR ( 'NONE', #1652, 1000.000000000000000 ) ;
#20931 = CARTESIAN_POINT ( 'NONE',  ( 0.000000000000000000, 1.999999999999998224, -126.0000000000000000 ) ) ;
#20932 = CIRCLE ( 'NONE', #1850, 4.000000000000002665 ) ;
#20933 = VECTOR ( 'NONE', #17083, 1000.000000000000000 ) ;
#20934 = LINE ( 'NONE', #10500, #19851 ) ;
#20935 = ORIENTED_EDGE ( 'NONE', *, *, #17685, .T. ) ;
#20936 = DIRECTION ( 'NONE',  ( 0.9506032891036972909, -0.3102281881984320644, -0.01057629388542894074 ) ) ;
#20937 = ORIENTED_EDGE ( 'NONE', *, *, #3304, .T. ) ;
#20938 = DIRECTION ( 'NONE',  ( 0.9934404589540162256, 0.1135548637187056842, -0.01346653032743081423 ) ) ;
#20939 = AXIS2_PLACEMENT_3D ( 'NONE', #660, #22293, #1213 ) ;
#20941 = ORIENTED_EDGE ( 'NONE', *, *, #16162, .F. ) ;
#20940 = ORIENTED_EDGE ( 'NONE', *, *, #10203, .F. ) ;
#20942 = CARTESIAN_POINT ( 'NONE',  ( 164.0000000000000000, 20.00000000000000000, 2.250243343269062756E-12 ) ) ;
#20943 = CARTESIAN_POINT ( 'NONE',  ( 92.43457499998882554, 77.12912189496645965, -31.19724316448930423 ) ) ;
#20944 = DIRECTION ( 'NONE',  ( -0.1296504907605101897, -0.005475273188901850878, -0.9915446392518421082 ) ) ;
#20945 = FACE_OUTER_BOUND ( 'NONE', #2000, .T. ) ;
#20946 = AXIS2_PLACEMENT_3D ( 'NONE', #258, #5521, #9320 ) ;
#20947 = SURFACE_SIDE_STYLE ('',( #6825 ) ) ;
#20948 = DIRECTION ( 'NONE',  ( -0.01292394549866632963, -0.005513023399716958026, -0.9999012842304692006 ) ) ;
#20949 = CIRCLE ( 'NONE', #3720, 1.999999999999998224 ) ;
#20950 = CARTESIAN_POINT ( 'NONE',  ( 0.000000000000000000, 25.00000000000000000, 118.0000000000000000 ) ) ;
#20951 = CARTESIAN_POINT ( 'NONE',  ( -93.21002351426726307, 77.12912189496638860, -28.79774562292281104 ) ) ;
#20952 = CARTESIAN_POINT ( 'NONE',  ( 48.53901525512552695, 159.4173909239030706, 268.0562281683617130 ) ) ;
#20953 = ORIENTED_EDGE ( 'NONE', *, *, #18395, .T. ) ;
#20954 = AXIS2_PLACEMENT_3D ( 'NONE', #16153, #21392, #17876 ) ;
#20955 = DIRECTION ( 'NONE',  ( -7.176269450075762180E-19, 1.000000000000000000, -5.550596000020001457E-17 ) ) ;
#20956 = CARTESIAN_POINT ( 'NONE',  ( -3.606137745152995233, 157.2416648407696016, 299.7452723209433998 ) ) ;
#20957 = ORIENTED_EDGE ( 'NONE', *, *, #4242, .T. ) ;
#20959 = CARTESIAN_POINT ( 'NONE',  ( -91.69412133380704688, 80.03889463956294037, -29.36066737363279699 ) ) ;
#20958 = AXIS2_PLACEMENT_3D ( 'NONE', #1298, #18614, #6342 ) ;
#20960 = EDGE_LOOP ( 'NONE', ( #16142, #16776, #2572, #6116, #1460 ) ) ;
#20961 = AXIS2_PLACEMENT_3D ( 'NONE', #18980, #3024, #18872 ) ;
#20962 = VECTOR ( 'NONE', #11952, 1000.000000000000000 ) ;
#20963 = CARTESIAN_POINT ( 'NONE',  ( 44.91100620407951993, 166.8507685304810764, 256.0609518519894436 ) ) ;
#20964 = CIRCLE ( 'NONE', #3383, 4.199999999999997513 ) ;
#20965 = DIRECTION ( 'NONE',  ( -0.9916643202943333790, 7.114886815082618290E-18, -0.1288482667915160917 ) ) ;
#20966 = FACE_OUTER_BOUND ( 'NONE', #17540, .T. ) ;
#20967 = FILL_AREA_STYLE ('',( #6953 ) ) ;
#20968 = CARTESIAN_POINT ( 'NONE',  ( 20.09393204039708181, 146.8369376497900021, 276.4047955799927081 ) ) ;
#20969 = ORIENTED_EDGE ( 'NONE', *, *, #637, .F. ) ;
#20970 = CARTESIAN_POINT ( 'NONE',  ( 12.37946041904351446, 187.6360129020394254, 322.9658423925303055 ) ) ;
#20971 = ORIENTED_EDGE ( 'NONE', *, *, #235, .F. ) ;
#20972 = AXIS2_PLACEMENT_3D ( 'NONE', #8647, #5083, #12118 ) ;
#20973 = LINE ( 'NONE', #19133, #9707 ) ;
#20974 = EDGE_CURVE ( 'NONE', #12496, #16244, #20732, .T. ) ;
#20975 = AXIS2_PLACEMENT_3D ( 'NONE', #8588, #16086, #5247 ) ;
#20976 = VECTOR ( 'NONE', #13768, 1000.000000000000000 ) ;
#20977 = DIRECTION ( 'NONE',  ( 0.3102455404053341415, 0.9506564598521393128, 0.000000000000000000 ) ) ;
#20978 = VERTEX_POINT ( 'NONE', #22536 ) ;
#20979 = CARTESIAN_POINT ( 'NONE',  ( -10.92051603998877773, 183.4567045018018518, 323.0038140145950933 ) ) ;
#20980 = FACE_OUTER_BOUND ( 'NONE', #7498, .T. ) ;
#20981 = ORIENTED_EDGE ( 'NONE', *, *, #7109, .F. ) ;
#20982 = CARTESIAN_POINT ( 'NONE',  ( -44.72589015212603414, 164.7311077213657597, 273.2327950865263801 ) ) ;
#20983 = ORIENTED_EDGE ( 'NONE', *, *, #8209, .F. ) ;
#20984 = DIRECTION ( 'NONE',  ( 0.01292394549866739996, 0.005513023399721131770, 0.9999012842304692006 ) ) ;
#20985 = VECTOR ( 'NONE', #5978, 999.9999999999998863 ) ;
#20986 = CARTESIAN_POINT ( 'NONE',  ( -10.85567112094788200, 105.6999953372425551, 127.2994028633183348 ) ) ;
#20987 = FACE_OUTER_BOUND ( 'NONE', #10431, .T. ) ;
#20988 =( REPRESENTATION_RELATIONSHIP ('NONE','NONE', #11808, #3137 ) REPRESENTATION_RELATIONSHIP_WITH_TRANSFORMATION ( #17344 )SHAPE_REPRESENTATION_RELATIONSHIP( ) );
#20989 = CARTESIAN_POINT ( 'NONE',  ( 17.48759048301047869, 184.6901107042388048, 307.3088310089726747 ) ) ;
#20990 = EDGE_CURVE ( 'NONE', #555, #17192, #20831, .T. ) ;
#20991 = DIRECTION ( 'NONE',  ( 5.440186201345738641E-18, 1.000000000000000000, 1.334940939666364181E-17 ) ) ;
#20992 = ORIENTED_EDGE ( 'NONE', *, *, #9145, .T. ) ;
#20993 = AXIS2_PLACEMENT_3D ( 'NONE', #13093, #22113, #9391 ) ;
#20994 = CARTESIAN_POINT ( 'NONE',  ( 43.22177362078638652, 125.3750519639578727, 249.0040540354910092 ) ) ;
#20995 = CIRCLE ( 'NONE', #4484, 2.000000000000001776 ) ;
#20996 = DIRECTION ( 'NONE',  ( 7.125109674161246868E-05, -0.9999848031710253382, 0.005512562950850155054 ) ) ;
#20997 = EDGE_CURVE ( 'NONE', #11742, #6632, #5283, .T. ) ;
#20998 = LINE ( 'NONE', #8363, #6355 ) ;
#20999 = DIRECTION ( 'NONE',  ( -0.7944560844389302323, 1.242937374672305755E-17, -0.6073216033519337476 ) ) ;
#21000 = LINE ( 'NONE', #15982, #20547 ) ;
#21001 = CIRCLE ( 'NONE', #11122, 8.000000000000003553 ) ;
#21002 = CARTESIAN_POINT ( 'NONE',  ( 0.000000000000000000, 0.000000000000000000, 124.0000000000000000 ) ) ;
#21003 = EDGE_CURVE ( 'NONE', #10899, #7432, #8957, .T. ) ;
#21004 = VERTEX_POINT ( 'NONE', #520 ) ;
#21005 = DIRECTION ( 'NONE',  ( 0.9909299940865188283, -0.1338359446631172955, -0.01207007604876047212 ) ) ;
#21006 = ADVANCED_FACE ( 'NONE', ( #21402 ), #15812, .T. ) ;
#21007 = CARTESIAN_POINT ( 'NONE',  ( 51.06003536384874053, 189.6011917897851333, -73.05933252543843537 ) ) ;
#21008 = ORIENTED_EDGE ( 'NONE', *, *, #2, .T. ) ;
#21009 = EDGE_CURVE ( 'NONE', #20773, #8421, #19232, .T. ) ;
#21010 = CARTESIAN_POINT ( 'NONE',  ( 49.56102085612021568, 109.7790983012155834, -47.31406271648155837 ) ) ;
#21011 = ORIENTED_EDGE ( 'NONE', *, *, #18029, .F. ) ;
#21012 = ADVANCED_FACE ( 'NONE', ( #17771 ), #13689, .T. ) ;
#21013 = CARTESIAN_POINT ( 'NONE',  ( -10.43449472670604550, 70.35701968572537623, -92.68424618042337215 ) ) ;
#21014 = CARTESIAN_POINT ( 'NONE',  ( 1.028703311283776507E-14, 0.000000000000000000, 83.99999999999998579 ) ) ;
#21015 = DIRECTION ( 'NONE',  ( 0.9999164797902015955, 2.045733645417851681E-15, -0.01292414190464156835 ) ) ;
#21016 = AXIS2_PLACEMENT_3D ( 'NONE', #8541, #22426, #1339 ) ;
#21017 = EDGE_CURVE ( 'NONE', #11382, #9044, #7872, .T. ) ;
#21018 = CIRCLE ( 'NONE', #9667, 6.499999999999998224 ) ;
#21019 = DIRECTION ( 'NONE',  ( 0.000000000000000000, 1.000000000000000000, 0.000000000000000000 ) ) ;
#21020 = FACE_OUTER_BOUND ( 'NONE', #10634, .T. ) ;
#21021 = ORIENTED_EDGE ( 'NONE', *, *, #8252, .F. ) ;
#21022 = CARTESIAN_POINT ( 'NONE',  ( 0.005291762159211760297, 327.3029031209191544, 311.7951952913599030 ) ) ;
#21023 = EDGE_CURVE ( 'NONE', #20688, #10848, #747, .T. ) ;
#21024 = CARTESIAN_POINT ( 'NONE',  ( -36.77797314829808784, 121.7015652700167152, 249.5406332993740648 ) ) ;
#21025 = ORIENTED_EDGE ( 'NONE', *, *, #16325, .F. ) ;
#21026 = AXIS2_PLACEMENT_3D ( 'NONE', #5210, #7393, #17768 ) ;
#21027 = CARTESIAN_POINT ( 'NONE',  ( -10.43449472670604372, 81.64298031427460955, -92.68424618042337215 ) ) ;
#21028 = CARTESIAN_POINT ( 'NONE',  ( -89.76607547520649177, 88.98826100381097604, 52.04949514552107814 ) ) ;
#21029 = EDGE_CURVE ( 'NONE', #11795, #22165, #2247, .T. ) ;
#21030 = AXIS2_PLACEMENT_3D ( 'NONE', #22088, #17080, #18886 ) ;
#21032 = ORIENTED_EDGE ( 'NONE', *, *, #10075, .F. ) ;
#21031 = ORIENTED_EDGE ( 'NONE', *, *, #19692, .T. ) ;
#21033 = AXIS2_PLACEMENT_3D ( 'NONE', #8648, #5320, #3381 ) ;
#21034 = ORIENTED_EDGE ( 'NONE', *, *, #14610, .T. ) ;
#21035 = CARTESIAN_POINT ( 'NONE',  ( 1.469576158976823671E-14, 25.00000000000000000, 120.0000000000000000 ) ) ;
#21036 = CARTESIAN_POINT ( 'NONE',  ( 3.622049127414185499, 188.3056765838590252, 296.4802766975643635 ) ) ;
#21037 = CARTESIAN_POINT ( 'NONE',  ( 85.05181457928490829, 75.00176059250011917, -1.764877938563226500 ) ) ;
#21038 = CARTESIAN_POINT ( 'NONE',  ( -146.5000000000000000, 20.00000000000000000, 10.00000000000002487 ) ) ;
#21039 = ORIENTED_EDGE ( 'NONE', *, *, #4431, .F. ) ;
#21040 = EDGE_CURVE ( 'NONE', #12722, #17081, #2803, .T. ) ;
#21041 = CARTESIAN_POINT ( 'NONE',  ( 14.35565316234159816, 188.7518249220741495, 275.4952485672711191 ) ) ;
#21042 = ORIENTED_EDGE ( 'NONE', *, *, #12739, .F. ) ;
#21043 = CYLINDRICAL_SURFACE ( 'NONE', #11533, 3.399999999999985700 ) ;
#21044 = AXIS2_PLACEMENT_3D ( 'NONE', #4692, #13241, #11725 ) ;
#21045 = CARTESIAN_POINT ( 'NONE',  ( -75.07425674568773388, 75.00865516402794242, -0.3536922578719212118 ) ) ;
#21046 = CARTESIAN_POINT ( 'NONE',  ( -26.63628795331713661, 324.2466416883012812, 309.4292525024184215 ) ) ;
#21047 = DIRECTION ( 'NONE',  ( -0.01292394549866731669, -0.005513023399720593139, -0.9999012842304692006 ) ) ;
#21048 = ORIENTED_EDGE ( 'NONE', *, *, #10556, .T. ) ;
#21049 = CARTESIAN_POINT ( 'NONE',  ( -37.04307294938801931, 93.86476689679389551, -82.35130986602069925 ) ) ;
#21050 = AXIS2_PLACEMENT_3D ( 'NONE', #20577, #9806, #8398 ) ;
#21051 = CARTESIAN_POINT ( 'NONE',  ( 105.4334892372614405, 72.00000000000000000, -31.36525700924962834 ) ) ;
#21052 = EDGE_LOOP ( 'NONE', ( #20050, #15413, #20030, #3731 ) ) ;
#21053 = AXIS2_PLACEMENT_3D ( 'NONE', #6980, #3536, #10548 ) ;
#21054 = CARTESIAN_POINT ( 'NONE',  ( -36.79739265342710297, 125.3640259171584290, 248.0381828194013849 ) ) ;
#21055 = ORIENTED_EDGE ( 'NONE', *, *, #15435, .F. ) ;
#21056 = ORIENTED_EDGE ( 'NONE', *, *, #3883, .F. ) ;
#21057 = CARTESIAN_POINT ( 'NONE',  ( 19.88808155476299433, 183.5654341500644193, 313.6124693336564633 ) ) ;
#21058 = ADVANCED_FACE ( 'NONE', ( #11082 ), #870, .F. ) ;
#21059 = VECTOR ( 'NONE', #20180, 999.9999999999998863 ) ;
#21061 = ORIENTED_EDGE ( 'NONE', *, *, #22183, .T. ) ;
#21060 = ORIENTED_EDGE ( 'NONE', *, *, #9581, .T. ) ;
#21062 = DIRECTION ( 'NONE',  ( -0.1337561903331544455, -0.9909881666746205298, 0.007192708699472569189 ) ) ;
#21063 = DIRECTION ( 'NONE',  ( -0.01292394549866738782, -0.005513023399720700692, -0.9999012842304693116 ) ) ;
#21064 = CARTESIAN_POINT ( 'NONE',  ( -10.88750796510622720, 109.6831336666334380, 124.2300622640541690 ) ) ;
#21065 = CONICAL_SURFACE ( 'NONE', #18499, 3.399999999999985700, 1.029744258676653201 ) ;
#21066 = AXIS2_PLACEMENT_3D ( 'NONE', #3182, #15180, #21897 ) ;
#21067 = CYLINDRICAL_SURFACE ( 'NONE', #21033, 2.499999999999988010 ) ;
#21068 = CARTESIAN_POINT ( 'NONE',  ( -38.90465531275731337, 97.20110498407991884, 83.98952174397253145 ) ) ;
#21069 = EDGE_LOOP ( 'NONE', ( #13935, #18407, #22015, #13224 ) ) ;
#21070 = DIRECTION ( 'NONE',  ( 0.9999164797902017066, 2.001050586450178931E-22, -0.01292414190464131508 ) ) ;
#21071 = DIRECTION ( 'NONE',  ( 0.9999164797902015955, 2.457859219970326020E-15, -0.01292414190464043211 ) ) ;
#21072 = CARTESIAN_POINT ( 'NONE',  ( 15.29795320234381251, 186.1234154815347779, 305.8048709493763226 ) ) ;
#21073 = CARTESIAN_POINT ( 'NONE',  ( 91.13609774473717096, 79.20914543161380550, 26.78943607724107423 ) ) ;
#21074 = CARTESIAN_POINT ( 'NONE',  ( -84.78539177974977292, 105.0000000000000000, -70.08164767436865361 ) ) ;
#21075 = AXIS2_PLACEMENT_3D ( 'NONE', #493, #5752, #9557 ) ;
#21076 = FACE_OUTER_BOUND ( 'NONE', #17150, .T. ) ;
#21077 = CARTESIAN_POINT ( 'NONE',  ( -162.0000000000000000, 18.00000000000000355, 53.76161406891260697 ) ) ;
#21078 = EDGE_LOOP ( 'NONE', ( #9025, #15843, #3574, #74 ) ) ;
#21079 = CARTESIAN_POINT ( 'NONE',  ( -92.06552853299464800, 79.93537922958711306, -29.07356135706641709 ) ) ;
#21080 = ORIENTED_EDGE ( 'NONE', *, *, #21659, .T. ) ;
#21081 = AXIS2_PLACEMENT_3D ( 'NONE', #16264, #8875, #19443 ) ;
#21082 = EDGE_CURVE ( 'NONE', #16057, #5358, #13155, .T. ) ;
#21083 = ADVANCED_FACE ( 'NONE', ( #9708 ), #18309, .T. ) ;
#21084 = FACE_BOUND ( 'NONE', #16863, .T. ) ;
#21085 = B_SPLINE_CURVE_WITH_KNOTS ( 'NONE', 3,
 ( #3027, #15571, #6486, #20369, #13398, #4631, #3139, #10156, #10264, #13727 ),
 .UNSPECIFIED., .F., .F.,
 ( 4, 2, 2, 2, 4 ),
 ( 0.000000000000000000, 0.002118048795477085657, 0.003177073193215628269, 0.003706585392084899792, 0.004236097590954171314 ),
 .UNSPECIFIED. ) ;
#21086 = CARTESIAN_POINT ( 'NONE',  ( 1.175660927181459158E-14, 37.00000000000000711, 96.00000000000000000 ) ) ;
#21087 = PLANE ( 'NONE',  #6003 ) ;
#21088 = DIRECTION ( 'NONE',  ( -0.01292394549866740169, -0.005513023399721063249, -0.9999012842304692006 ) ) ;
#21089 = EDGE_LOOP ( 'NONE', ( #14692, #14276, #20390, #21943 ) ) ;
#21090 = CARTESIAN_POINT ( 'NONE',  ( 12.91603429844997741, 190.3480582277193776, 320.8611997870096388 ) ) ;
#21091 = EDGE_LOOP ( 'NONE', ( #2145, #1740, #19399, #11154 ) ) ;
#21092 = FACE_OUTER_BOUND ( 'NONE', #14019, .T. ) ;
#21093 = CARTESIAN_POINT ( 'NONE',  ( 71.06083360305758845, 91.87225009003579146, 83.96645210693642980 ) ) ;
#21094 = FILL_AREA_STYLE ('',( #2036 ) ) ;
#21095 = FACE_OUTER_BOUND ( 'NONE', #18773, .T. ) ;
#21096 = CARTESIAN_POINT ( 'NONE',  ( -92.40872671617950118, 69.99999999999998579, 33.19707612406966746 ) ) ;
#21097 = ORIENTED_EDGE ( 'NONE', *, *, #5007, .F. ) ;
#21098 = CARTESIAN_POINT ( 'NONE',  ( -14.84893071567995904, 180.4293321838713666, 312.3514243336252889 ) ) ;
#21099 = CARTESIAN_POINT ( 'NONE',  ( -56.88925295215435085, 118.2576901802692646, 47.62393161023230448 ) ) ;
#21100 = FACE_OUTER_BOUND ( 'NONE', #16256, .T. ) ;
#21101 = CARTESIAN_POINT ( 'NONE',  ( -15.38762379257795665, 178.0062715105021312, 316.6788287982297447 ) ) ;
#21102 = VECTOR ( 'NONE', #9649, 1000.000000000000000 ) ;
#21103 = ORIENTED_EDGE ( 'NONE', *, *, #1441, .F. ) ;
#21104 = B_SPLINE_CURVE_WITH_KNOTS ( 'NONE', 3,
 ( #18405, #22265, #13364, #15317, #20444, #4816, #4487, #3109 ),
 .UNSPECIFIED., .F., .F.,
 ( 4, 2, 2, 4 ),
 ( 0.002921158035944515681, 0.003648658618861458543, 0.004376159201778400537, 0.005831160367612286261 ),
 .UNSPECIFIED. ) ;
#21105 = EDGE_CURVE ( 'NONE', #22542, #848, #13646, .T. ) ;
#21106 = CARTESIAN_POINT ( 'NONE',  ( 11.85964614693714836, 187.7423844643599296, 304.8777488482054423 ) ) ;
#21107 = PLANE ( 'NONE',  #19953 ) ;
#21108 = CARTESIAN_POINT ( 'NONE',  ( -37.56383571331804916, 165.5072604488013326, 268.7355101842127283 ) ) ;
#21109 = EDGE_CURVE ( 'NONE', #1394, #10157, #19096, .T. ) ;
#21110 = CARTESIAN_POINT ( 'NONE',  ( -45.15312007873932032, 180.5703843163154261, 257.1494065962392597 ) ) ;
#21111 = CONTEXT_DEPENDENT_SHAPE_REPRESENTATION ( #10002, #15827 ) ;
#21112 = CARTESIAN_POINT ( 'NONE',  ( -74.89374433628610461, 54.99999999999999289, 0.9680182286576737294 ) ) ;
#21113 = CARTESIAN_POINT ( 'NONE',  ( -36.23709397917757258, 94.19957547782705376, 83.27571307199862360 ) ) ;
#21114 = DIRECTION ( 'NONE',  ( 0.9909299940865186063, -0.1338359446631180727, -0.01207007604876311237 ) ) ;
#21115 = CARTESIAN_POINT ( 'NONE',  ( -47.96343107302703146, 166.9147430771239442, 269.2622064964168658 ) ) ;
#21116 = DIRECTION ( 'NONE',  ( 0.000000000000000000, 1.000000000000000000, 0.000000000000000000 ) ) ;
#21117 = CARTESIAN_POINT ( 'NONE',  ( 9.674709713264089326E-15, 29.00000000000000711, 78.99999999999998579 ) ) ;
#21118 = VECTOR ( 'NONE', #18489, 999.9999999999998863 ) ;
#21119 = ORIENTED_EDGE ( 'NONE', *, *, #5894, .F. ) ;
#21120 = CARTESIAN_POINT ( 'NONE',  ( -66.42677970909001317, 189.3893605493459233, -109.9672025422466959 ) ) ;
#21121 = PRODUCT_DEFINITION_SHAPE ( 'NONE', 'NONE',  #22668 ) ;
#21122 = CARTESIAN_POINT ( 'NONE',  ( -38.68617183816869698, 163.9153776386440882, 273.1592279730091377 ) ) ;
#21123 = EDGE_CURVE ( 'NONE', #10917, #20879, #6900, .T. ) ;
#21124 = ORIENTED_EDGE ( 'NONE', *, *, #2884, .F. ) ;
#21125 = DIRECTION ( 'NONE',  ( 0.8981428216241997831, -0.000000000000000000, 0.4397038457472493556 ) ) ;
#21126 = ORIENTED_EDGE ( 'NONE', *, *, #15505, .T. ) ;
#21127 = CARTESIAN_POINT ( 'NONE',  ( 13.28235005706528682, 159.1720975239875884, 299.5163413053770682 ) ) ;
#21128 = DIRECTION ( 'NONE',  ( -5.440186201345738641E-18, -1.000000000000000000, -1.334940939666364181E-17 ) ) ;
#21129 = DIRECTION ( 'NONE',  ( -0.8077751305149004635, -0.4220031449644254806, -0.4115977212786404160 ) ) ;
#21130 = APPLICATION_CONTEXT ( 'automotive_design' ) ;
#21131 = EDGE_LOOP ( 'NONE', ( #18591, #13918, #3988, #6044 ) ) ;
#21132 = PLANE ( 'NONE',  #1961 ) ;
#21133 = PRESENTATION_STYLE_ASSIGNMENT (( #22593 ) ) ;
#21134 = DIRECTION ( 'NONE',  ( -0.009088227368119913829, -0.7109943316365106014, -0.7031390079522376046 ) ) ;
#21135 = CARTESIAN_POINT ( 'NONE',  ( 16.02863756297163178, 168.1280733087994577, 320.9370496218247126 ) ) ;
#21136 = VERTEX_POINT ( 'NONE', #20017 ) ;
#21137 = ADVANCED_FACE ( 'NONE', ( #11305 ), #8846, .F. ) ;
#21138 = DIRECTION ( 'NONE',  ( -0.01292414190464023262, 0.000000000000000000, -0.9999164797902017066 ) ) ;
#21139 = CARTESIAN_POINT ( 'NONE',  ( -89.93251366689203508, 88.82716965768310047, 52.34818047611932457 ) ) ;
#21140 = ADVANCED_FACE ( 'NONE', ( #16727 ), #976, .T. ) ;
#21141 = PRODUCT ( 'Upper Movable Jaw Swivel Housing', 'Upper Movable Jaw Swivel Housing', '', ( #1279 ) ) ;
#21143 = ORIENTED_EDGE ( 'NONE', *, *, #10071, .T. ) ;
#21142 = ORIENTED_EDGE ( 'NONE', *, *, #9920, .T. ) ;
#21144 = ORIENTED_EDGE ( 'NONE', *, *, #17041, .T. ) ;
#21145 = DIRECTION ( 'NONE',  ( 0.01292394549866737220, 0.005513023399721000799, 0.9999012842304692006 ) ) ;
#21146 = CARTESIAN_POINT ( 'NONE',  ( 79.92740525950247843, 75.13699351169599083, -6.133505399301336425 ) ) ;
#21147 = CARTESIAN_POINT ( 'NONE',  ( 35.95309506732430549, 93.50464841319750064, 82.03286182426640494 ) ) ;
#21148 = EDGE_CURVE ( 'NONE', #5655, #922, #4843, .T. ) ;
#21149 = ORIENTED_EDGE ( 'NONE', *, *, #10201, .F. ) ;
#21150 = CARTESIAN_POINT ( 'NONE',  ( 18.17462290198324126, 185.9111733914936053, 277.9589104919019746 ) ) ;
#21151 = EDGE_LOOP ( 'NONE', ( #18146, #9780 ) ) ;
#21152 = CARTESIAN_POINT ( 'NONE',  ( 39.75021781620444727, 69.99999999999998579, 86.03367798009509215 ) ) ;
#21153 = DIRECTION ( 'NONE',  ( 0.01292394549866740169, 0.005513023399720822990, 0.9999012842304693116 ) ) ;
#21154 = CARTESIAN_POINT ( 'NONE',  ( -64.99457118636313169, 170.0000000000000284, 0.8400692238016805868 ) ) ;
#21155 = CARTESIAN_POINT ( 'NONE',  ( -26.93345542666578751, 324.2139270369915494, 309.7437723479166607 ) ) ;
#21156 = VERTEX_POINT ( 'NONE', #6803 ) ;
#21157 = CARTESIAN_POINT ( 'NONE',  ( -64.99143613810649356, 126.0006686604749291, 1.082621993639087288 ) ) ;
#21158 = EDGE_CURVE ( 'NONE', #18692, #1423, #10039, .T. ) ;
#21159 = EDGE_LOOP ( 'NONE', ( #9923, #16054, #14676, #12950 ) ) ;
#21160 = FACE_OUTER_BOUND ( 'NONE', #15589, .T. ) ;
#21161 = FILL_AREA_STYLE ('',( #14183 ) ) ;
#21162 = CARTESIAN_POINT ( 'NONE',  ( 105.3515605809559048, 70.97896074530382293, -31.63944816216644185 ) ) ;
#21163 = ORIENTED_EDGE ( 'NONE', *, *, #22347, .T. ) ;
#21164 = VERTEX_POINT ( 'NONE', #22189 ) ;
#21165 = DIRECTION ( 'NONE',  ( 0.000000000000000000, -1.000000000000000000, 0.000000000000000000 ) ) ;
#21166 = ORIENTED_EDGE ( 'NONE', *, *, #6824, .F. ) ;
#21167 = EDGE_LOOP ( 'NONE', ( #10561, #685, #20223, #19067, #3197, #12770 ) ) ;
#21168 = ORIENTED_EDGE ( 'NONE', *, *, #5139, .T. ) ;
#21169 = DIRECTION ( 'NONE',  ( 0.3101392564284315978, 0.9506461370142478273, -0.009250070373106959384 ) ) ;
#21170 = EDGE_CURVE ( 'NONE', #6519, #2719, #20949, .T. ) ;
#21171 = ORIENTED_EDGE ( 'NONE', *, *, #17629, .F. ) ;
#21172 = CIRCLE ( 'NONE', #4290, 2.000000000000000000 ) ;
#21173 = CARTESIAN_POINT ( 'NONE',  ( 92.28892611776127808, 77.12912189496647386, -31.19536062043667357 ) ) ;
#21174 = CARTESIAN_POINT ( 'NONE',  ( -91.17321230992149594, 70.18788889246519602, 61.54298701807832828 ) ) ;
#21175 = CARTESIAN_POINT ( 'NONE',  ( -1.163172771417702700, 37.00000000000000711, -89.99248318111824574 ) ) ;
#21176 = CARTESIAN_POINT ( 'NONE',  ( -38.92003986412552052, 97.39926864640102622, 83.81297216957182172 ) ) ;
#21177 = SHAPE_REPRESENTATION ( 'Flange', ( #6292 ), #21305 ) ;
#21178 = SURFACE_STYLE_FILL_AREA ( #12584 ) ;
#21179 = CARTESIAN_POINT ( 'NONE',  ( 77.15497946248154904, 75.16563907528397692, -6.606045424387566811 ) ) ;
#21180 = CARTESIAN_POINT ( 'NONE',  ( 17.20553148001535604, 184.8947804991583155, 307.0627613442703137 ) ) ;
#21181 = CARTESIAN_POINT ( 'NONE',  ( 91.85896106039241715, 79.10764833873324164, 26.44817522613584515 ) ) ;
#21182 = DIRECTION ( 'NONE',  ( -0.01292394549866731843, -0.005513023399720594006, -0.9999012842304693116 ) ) ;
#21183 = ADVANCED_FACE ( 'NONE', ( #11761 ), #11990, .F. ) ;
#21184 = VECTOR ( 'NONE', #16912, 1000.000000000000000 ) ;
#21185 = DIRECTION ( 'NONE',  ( -0.01292414190464131508, -1.902755938799530474E-22, -0.9999164797902017066 ) ) ;
#21186 = AXIS2_PLACEMENT_3D ( 'NONE', #1823, #8815, #6652 ) ;
#21187 = CARTESIAN_POINT ( 'NONE',  ( 1.168872497073783157, 177.4987173824078468, 90.43346020349439129 ) ) ;
#21188 = ORIENTED_EDGE ( 'NONE', *, *, #7129, .T. ) ;
#21189 = LINE ( 'NONE', #5443, #7629 ) ;
#21190 = EDGE_LOOP ( 'NONE', ( #14616, #20755, #10754 ) ) ;
#21191 = EDGE_CURVE ( 'NONE', #16857, #8492, #22222, .T. ) ;
#21192 = EDGE_CURVE ( 'NONE', #9610, #2301, #21666, .T. ) ;
#21193 = DIRECTION ( 'NONE',  ( 0.9999164797902015955, 2.001050586450178695E-22, -0.01292414190464131335 ) ) ;
#21194 = LINE ( 'NONE', #5448, #17565 ) ;
#21195 = CARTESIAN_POINT ( 'NONE',  ( -7.475646132950445555, 70.80384757729335377, -81.73701953211951832 ) ) ;
#21196 = STYLED_ITEM ( 'NONE', ( #19247 ), #1836 ) ;
#21197 = DIRECTION ( 'NONE',  ( 0.9999164797902015955, 0.000000000000000000, -0.01292414190463754553 ) ) ;
#21198 = ORIENTED_EDGE ( 'NONE', *, *, #1271, .T. ) ;
#21199 = DIRECTION ( 'NONE',  ( -0.009760756503428009989, 0.9999378516499564107, -0.005387065077611111891 ) ) ;
#21200 = VERTEX_POINT ( 'NONE', #15451 ) ;
#21201 = FACE_OUTER_BOUND ( 'NONE', #5828, .T. ) ;
#21202 = CARTESIAN_POINT ( 'NONE',  ( 71.00742074342186072, 91.74173777283633058, 84.01159762260415675 ) ) ;
#21203 = EDGE_CURVE ( 'NONE', #6548, #13285, #8407, .T. ) ;
#21204 = CARTESIAN_POINT ( 'NONE',  ( -9.825094046574873730, 187.6899473416463309, 321.1602656712647104 ) ) ;
#21205 = EDGE_CURVE ( 'NONE', #22007, #10601, #418, .T. ) ;
#21206 = CARTESIAN_POINT ( 'NONE',  ( -88.41758806590422637, 80.31838830481380853, 32.48564084813593666 ) ) ;
#21207 = CARTESIAN_POINT ( 'NONE',  ( -164.0000000000000000, 18.00000000000000355, -7.999999999999979572 ) ) ;
#21208 = ORIENTED_EDGE ( 'NONE', *, *, #16113, .T. ) ;
#21209 = VECTOR ( 'NONE', #7627, 1000.000000000000000 ) ;
#21210 = CARTESIAN_POINT ( 'NONE',  ( -10.33748581482210938, 187.5699477589057835, 308.1934098357545508 ) ) ;
#21211 = DIRECTION ( 'NONE',  ( -0.9999164797902015955, -4.476705744456278510E-15, 0.01292414190464144692 ) ) ;
#21212 = CARTESIAN_POINT ( 'NONE',  ( -4.597416034112115746, 326.7591350836430593, 307.4820788455573961 ) ) ;
#21213 = CARTESIAN_POINT ( 'NONE',  ( -14.02470704512671773, 182.1275625653396162, 318.7217756528992254 ) ) ;
#21214 = CARTESIAN_POINT ( 'NONE',  ( 13.09166901539544803, 187.2406732805667389, 305.0407694685882802 ) ) ;
#21215 = VERTEX_POINT ( 'NONE', #8204 ) ;
#21216 = FACE_OUTER_BOUND ( 'NONE', #21312, .T. ) ;
#21217 = CONTEXT_DEPENDENT_SHAPE_REPRESENTATION ( #16203, #6809 ) ;
#21218 = CARTESIAN_POINT ( 'NONE',  ( 39.10370113529218372, 92.00280690327063837, 83.45957852174062452 ) ) ;
#21219 = AXIS2_PLACEMENT_3D ( 'NONE', #22539, #18791, #10073 ) ;
#21220 = LINE ( 'NONE', #12403, #17362 ) ;
#21221 = CARTESIAN_POINT ( 'NONE',  ( -1.124400345703781001, 69.99999999999998579, -86.99273374174757123 ) ) ;
#21222 = MECHANICAL_DESIGN_GEOMETRIC_PRESENTATION_REPRESENTATION (  '', ( #10238 ), #14290 ) ;
#21223 = CARTESIAN_POINT ( 'NONE',  ( 50.99361748650641601, 111.8657007576893960, -48.09684511357723835 ) ) ;
#21224 = VERTEX_POINT ( 'NONE', #8629 ) ;
#21225 = CARTESIAN_POINT ( 'NONE',  ( -54.77086557510170906, 114.8307698053962156, 171.9727639297506414 ) ) ;
#21226 = FACE_OUTER_BOUND ( 'NONE', #15847, .T. ) ;
#21227 = ORIENTED_EDGE ( 'NONE', *, *, #11185, .F. ) ;
#21228 = CARTESIAN_POINT ( 'NONE',  ( -49.26352808811260786, 95.06875159149220167, -43.57455600632292914 ) ) ;
#21229 = ORIENTED_EDGE ( 'NONE', *, *, #21205, .F. ) ;
#21231 = DIRECTION ( 'NONE',  ( 7.125109674141484573E-05, -0.9999848031710252272, 0.005512562950851785694 ) ) ;
#21230 = FACE_OUTER_BOUND ( 'NONE', #20900, .T. ) ;
#21232 = CARTESIAN_POINT ( 'NONE',  ( 0.000000000000000000, 45.00000000000000000, 110.1134477342067157 ) ) ;
#21233 = DIRECTION ( 'NONE',  ( -0.9999464000778708339, -1.417269118681874529E-05, 0.01035358732233823860 ) ) ;
#21234 = CARTESIAN_POINT ( 'NONE',  ( 11.27670803124779297, 143.4306312998254214, 275.5969523110588284 ) ) ;
#21235 = CIRCLE ( 'NONE', #4363, 110.0000000000000142 ) ;
#21236 = CARTESIAN_POINT ( 'NONE',  ( 21.87694519636252366, 168.7662676875228556, 313.3507060617185402 ) ) ;
#21237 = VECTOR ( 'NONE', #9, 1000.000000000000114 ) ;
#21238 = ORIENTED_EDGE ( 'NONE', *, *, #12170, .T. ) ;
#21239 = CARTESIAN_POINT ( 'NONE',  ( 51.87369047120967025, 152.9724930639170282, 274.1190593707768812 ) ) ;
#21240 = EDGE_CURVE ( 'NONE', #12967, #14863, #10744, .T. ) ;
#21241 = CARTESIAN_POINT ( 'NONE',  ( -89.97667839591423444, 87.76279617797230514, 50.93259715458368220 ) ) ;
#21242 = VERTEX_POINT ( 'NONE', #8305 ) ;
#21243 = ORIENTED_EDGE ( 'NONE', *, *, #5219, .F. ) ;
#21244 = DIRECTION ( 'NONE',  ( -2.025474946048326158E-22, 1.000000000000000000, -1.876735158486679638E-22 ) ) ;
#21245 = DIRECTION ( 'NONE',  ( 0.01292414190464131335, 1.902755938799530239E-22, 0.9999164797902015955 ) ) ;
#21246 = AXIS2_PLACEMENT_3D ( 'NONE', #5799, #19694, #10643 ) ;
#21247 = CARTESIAN_POINT ( 'NONE',  ( -106.1909711380429115, 71.47214965576930013, -28.69631340039675749 ) ) ;
#21248 = LINE ( 'NONE', #17386, #5630 ) ;
#21249 = ORIENTED_EDGE ( 'NONE', *, *, #21880, .T. ) ;
#21250 = CARTESIAN_POINT ( 'NONE',  ( 91.57598704441285520, 77.66227243743308861, 29.67486887243840954 ) ) ;
#21251 = ORIENTED_EDGE ( 'NONE', *, *, #4338, .F. ) ;
#21252 = PLANE ( 'NONE',  #7728 ) ;
#21253 = CIRCLE ( 'NONE', #1471, 2.000000000000004885 ) ;
#21254 = DIRECTION ( 'NONE',  ( 7.125109674403277385E-05, -0.9999848031710253382, 0.005512562950848281552 ) ) ;
#21255 = DIRECTION ( 'NONE',  ( -0.01292414190463830014, 0.000000000000000000, -0.9999164797902017066 ) ) ;
#21256 = CARTESIAN_POINT ( 'NONE',  ( -27.63336591784069896, 324.1648741128184952, 317.4228176935731085 ) ) ;
#21257 = EDGE_CURVE ( 'NONE', #14285, #20578, #19522, .T. ) ;
#21258 = ORIENTED_EDGE ( 'NONE', *, *, #3442, .T. ) ;
#21259 = EDGE_CURVE ( 'NONE', #16597, #3063, #7017, .T. ) ;
#21260 = DIRECTION ( 'NONE',  ( 7.125109674403837105E-05, -0.9999848031710252272, 0.005512562950847867821 ) ) ;
#21261 = DIRECTION ( 'NONE',  ( -0.8517085755015534332, 0.1186618397176080614, 0.5104036345990761170 ) ) ;
#21262 = CARTESIAN_POINT ( 'NONE',  ( -35.41327317553044907, 106.1692389898096280, 200.3757439048835920 ) ) ;
#21263 = EDGE_CURVE ( 'NONE', #5091, #22007, #1167, .T. ) ;
#21264 = CARTESIAN_POINT ( 'NONE',  ( -9.009919365157752935, 180.4221386788646271, 76.66529449372310978 ) ) ;
#21265 = ORIENTED_EDGE ( 'NONE', *, *, #13151, .F. ) ;
#21266 = DIRECTION ( 'NONE',  ( 0.000000000000000000, 0.000000000000000000, 1.000000000000000000 ) ) ;
#21267 = VERTEX_POINT ( 'NONE', #4725 ) ;
#21268 = VECTOR ( 'NONE', #15308, 1000.000000000000114 ) ;
#21269 = ORIENTED_EDGE ( 'NONE', *, *, #19887, .F. ) ;
#21270 = ADVANCED_FACE ( 'NONE', ( #20811 ), #18754, .T. ) ;
#21271 = CARTESIAN_POINT ( 'NONE',  ( 19.63457776109410702, 183.9216010738356886, 312.5996499687972232 ) ) ;
#21272 = EDGE_CURVE ( 'NONE', #5251, #6123, #22027, .T. ) ;
#21273 = PRODUCT_DEFINITION_FORMATION_WITH_SPECIFIED_SOURCE ( 'ANY', '', #16046, .NOT_KNOWN. ) ;
#21275 = ORIENTED_EDGE ( 'NONE', *, *, #18737, .T. ) ;
#21274 = ORIENTED_EDGE ( 'NONE', *, *, #584, .F. ) ;
#21276 = ADVANCED_FACE ( 'NONE', ( #10590 ), #12538, .T. ) ;
#21277 = CIRCLE ( 'NONE', #19812, 2.000000000000006217 ) ;
#21278 = CARTESIAN_POINT ( 'NONE',  ( -56.85872436582616274, 143.2710928180442522, 49.98587074703711153 ) ) ;
#21279 = FACE_OUTER_BOUND ( 'NONE', #16824, .T. ) ;
#21280 = PLANE ( 'NONE',  #10781 ) ;
#21281 = CARTESIAN_POINT ( 'NONE',  ( -38.90024297381467022, 95.59673886424684497, 82.77677384650711190 ) ) ;
#21282 = ORIENTED_EDGE ( 'NONE', *, *, #18540, .T. ) ;
#21283 = CARTESIAN_POINT ( 'NONE',  ( -86.79222083800951282, 104.3814432989690602, -67.58039954014913064 ) ) ;
#21284 = CARTESIAN_POINT ( 'NONE',  ( 74.97531732193478149, 75.07593137031709318, -4.781986851995010390 ) ) ;
#21285 = CARTESIAN_POINT ( 'NONE',  ( 16.43553195852968685, 185.4773513502461810, 308.6447355220632858 ) ) ;
#21286 = CARTESIAN_POINT ( 'NONE',  ( 92.62880990220415356, 79.84869560962943069, 28.85690742247621898 ) ) ;
#21287 = AXIS2_PLACEMENT_3D ( 'NONE', #12935, #2577, #19904 ) ;
#21288 = ADVANCED_FACE ( 'NONE', ( #606 ), #5749, .F. ) ;
#21289 = VECTOR ( 'NONE', #17312, 999.9999999999998863 ) ;
#21290 = ADVANCED_FACE ( 'NONE', ( #7939 ), #6101, .T. ) ;
#21291 = CARTESIAN_POINT ( 'NONE',  ( -83.58290648752343088, 104.4142135623730780, -71.51152175067954886 ) ) ;
#21292 = EDGE_CURVE ( 'NONE', #1068, #12626, #18943, .T. ) ;
#21293 = AXIS2_PLACEMENT_3D ( 'NONE', #11496, #593, #2762 ) ;
#21294 = EDGE_CURVE ( 'NONE', #6357, #8826, #6215, .T. ) ;
#21295 = CARTESIAN_POINT ( 'NONE',  ( -8.330024601187750122, 185.3742117612894447, 323.2535488253523681 ) ) ;
#21296 = AXIS2_PLACEMENT_3D ( 'NONE', #11207, #18217, #18435 ) ;
#21297 = DIRECTION ( 'NONE',  ( -5.440186201345785633E-18, -1.000000000000000000, -1.334940939666367878E-17 ) ) ;
#21298 = ORIENTED_EDGE ( 'NONE', *, *, #8111, .F. ) ;
#21299 = CARTESIAN_POINT ( 'NONE',  ( -89.59156723394222865, 79.74270461908911045, -28.48704982653686457 ) ) ;
#21300 = ORIENTED_EDGE ( 'NONE', *, *, #22270, .T. ) ;
#21301 = EDGE_CURVE ( 'NONE', #2309, #16120, #16248, .T. ) ;
#21302 = VECTOR ( 'NONE', #9817, 1000.000000000000227 ) ;
#21303 = CARTESIAN_POINT ( 'NONE',  ( -6.192786246109094783, 81.64368954560633540, -98.23155991399221421 ) ) ;
#21304 = EDGE_CURVE ( 'NONE', #21621, #7906, #14001, .T. ) ;
#21305 =( GEOMETRIC_REPRESENTATION_CONTEXT ( 3 ) GLOBAL_UNCERTAINTY_ASSIGNED_CONTEXT ( ( #40 ) ) GLOBAL_UNIT_ASSIGNED_CONTEXT ( ( #13566, #3201, #20780 ) ) REPRESENTATION_CONTEXT ( 'NONE', 'WORKASPACE' ) );
#21306 = CARTESIAN_POINT ( 'NONE',  ( -53.78951186480472302, 118.2576901802692788, 47.58386677032791567 ) ) ;
#21307 = AXIS2_PLACEMENT_3D ( 'NONE', #10028, #8392, #13920 ) ;
#21308 = CARTESIAN_POINT ( 'NONE',  ( -8.792471272935648230, 70.07756262466200781, -84.90096239309924897 ) ) ;
#21309 = DIRECTION ( 'NONE',  ( 0.6979091139780412290, -0.003898296230782321518, -0.7161757269782903501 ) ) ;
#21310 = ORIENTED_EDGE ( 'NONE', *, *, #693, .F. ) ;
#21311 = DIRECTION ( 'NONE',  ( 0.000000000000000000, 0.000000000000000000, 1.000000000000000000 ) ) ;
#21312 = EDGE_LOOP ( 'NONE', ( #13042, #19299, #2235 ) ) ;
#21313 = CARTESIAN_POINT ( 'NONE',  ( -40.94813932551373625, 95.97017003981163441, 82.42564028881616878 ) ) ;
#21314 = EDGE_CURVE ( 'NONE', #18985, #12945, #16598, .T. ) ;
#21315 = CARTESIAN_POINT ( 'NONE',  ( 19.43877198876942813, 177.6144908738019694, 111.1987526180507047 ) ) ;
#21316 = DIRECTION ( 'NONE',  ( -0.01292394549866739996, -0.005513023399721131770, -0.9999012842304692006 ) ) ;
#21317 = CARTESIAN_POINT ( 'NONE',  ( -88.94497886703045708, 79.67058643966740306, 30.57398350459251901 ) ) ;
#21318 = CARTESIAN_POINT ( 'NONE',  ( 92.40872671617952960, 72.00000000000000000, -33.19707612406970298 ) ) ;
#21319 = VERTEX_POINT ( 'NONE', #9324 ) ;
#21320 = DIRECTION ( 'NONE',  ( -0.01292394549866741557, -0.005513023399720270480, -0.9999012842304693116 ) ) ;
#21321 = AXIS2_PLACEMENT_3D ( 'NONE', #11179, #1516, #8182 ) ;
#21322 = ORIENTED_EDGE ( 'NONE', *, *, #15296, .T. ) ;
#21323 = ORIENTED_EDGE ( 'NONE', *, *, #13151, .T. ) ;
#21324 = DIRECTION ( 'NONE',  ( 7.125109674403276030E-05, -0.9999848031710252272, 0.005512562950848280685 ) ) ;
#21325 = CARTESIAN_POINT ( 'NONE',  ( 18.96584720174124783, 168.4155415818909205, 308.9361215159025278 ) ) ;
#21326 = CARTESIAN_POINT ( 'NONE',  ( -13.95945144365540536, 180.1360528412382394, 320.5617120762407808 ) ) ;
#21327 = AXIS2_PLACEMENT_3D ( 'NONE', #21799, #7927, #14959 ) ;
#21328 = CARTESIAN_POINT ( 'NONE',  ( -38.90567791675928078, 92.58578643762697880, 84.92412894573205051 ) ) ;
#21329 = AXIS2_PLACEMENT_3D ( 'NONE', #14429, #277, #7735 ) ;
#21330 = ORIENTED_EDGE ( 'NONE', *, *, #21294, .T. ) ;
#21331 = CARTESIAN_POINT ( 'NONE',  ( -11.46885069223597853, 81.19615242270661781, -91.33151364841882014 ) ) ;
#21332 = ADVANCED_FACE ( 'NONE', ( #489, #7491 ), #19754, .T. ) ;
#21333 = ADVANCED_FACE ( 'NONE', ( #11053, #13127 ), #5991, .F. ) ;
#21334 = VECTOR ( 'NONE', #10787, 1000.000000000000114 ) ;
#21335 = CARTESIAN_POINT ( 'NONE',  ( 161.9999999999992610, 20.00000000000000000, -53.76161406891482386 ) ) ;
#21336 = CARTESIAN_POINT ( 'NONE',  ( -1.163172771417702700, 69.99999999999998579, -89.99248318111824574 ) ) ;
#21337 = DIRECTION ( 'NONE',  ( 0.01292394549866738782, 0.005513023399720468239, 0.9999012842304692006 ) ) ;
#21338 = EDGE_LOOP ( 'NONE', ( #9570, #17929 ) ) ;
#21339 = CARTESIAN_POINT ( 'NONE',  ( 87.98413419613014241, 100.6041916471018851, -66.02114910964037620 ) ) ;
#21340 = DIRECTION ( 'NONE',  ( 0.9999164797902017066, 6.965998958219365988E-18, -0.01292414190464157356 ) ) ;
#21341 = LINE ( 'NONE', #5611, #14700 ) ;
#21342 = AXIS2_PLACEMENT_3D ( 'NONE', #2795, #11748, #1312 ) ;
#21343 = ORIENTED_EDGE ( 'NONE', *, *, #5705, .T. ) ;
#21344 = CARTESIAN_POINT ( 'NONE',  ( -69.95498757883834173, 89.03960924830867896, 69.18506932511724017 ) ) ;
#21345 = SHAPE_REPRESENTATION_RELATIONSHIP ( 'NONE' , 'NONE' ,  #14914, #10220 ) ;
#21346 = DIRECTION ( 'NONE',  ( -0.01292394549866741384, -0.005513023399721118760, -0.9999012842304692006 ) ) ;
#21347 = CARTESIAN_POINT ( 'NONE',  ( -1.163172771417702700, 69.99999999999998579, -89.99248318111824574 ) ) ;
#21348 = DIRECTION ( 'NONE',  ( 0.1351880940536943077, -0.9908129862407182298, 0.003715578404455049076 ) ) ;
#21349 = ORIENTED_EDGE ( 'NONE', *, *, #952, .T. ) ;
#21350 = DIRECTION ( 'NONE',  ( -0.01292394549866731669, -0.005513023399720593139, -0.9999012842304692006 ) ) ;
#21351 = AXIS2_PLACEMENT_3D ( 'NONE', #11665, #6495, #16965 ) ;
#21352 = AXIS2_PLACEMENT_3D ( 'NONE', #16854, #6162, #11797 ) ;
#21353 = LINE ( 'NONE', #16675, #22333 ) ;
#21354 = EDGE_LOOP ( 'NONE', ( #12654, #11428, #1837, #9238 ) ) ;
#21355 = CARTESIAN_POINT ( 'NONE',  ( -11.46885069223597853, 81.19615242270661781, -91.33151364841882014 ) ) ;
#21356 = CARTESIAN_POINT ( 'NONE',  ( -89.90957607858042877, 87.87157606449417813, 50.86550588853232568 ) ) ;
#21357 = ADVANCED_FACE ( 'NONE', ( #20216 ), #4362, .F. ) ;
#21358 = VECTOR ( 'NONE', #17122, 999.9999999999998863 ) ;
#21359 = PRODUCT_CONTEXT ( 'NONE', #12939, 'mechanical' ) ;
#21360 = ORIENTED_EDGE ( 'NONE', *, *, #3061, .T. ) ;
#21361 = ORIENTED_EDGE ( 'NONE', *, *, #4998, .F. ) ;
#21362 = CARTESIAN_POINT ( 'NONE',  ( 40.98661049262742750, 104.0316351437719362, 76.07369909541560560 ) ) ;
#21363 = DIRECTION ( 'NONE',  ( 0.000000000000000000, 0.000000000000000000, 1.000000000000000000 ) ) ;
#21364 = VECTOR ( 'NONE', #4555, 1000.000000000000114 ) ;
#21365 = DIRECTION ( 'NONE',  ( -0.9999164797902015955, -6.965998958219364448E-18, 0.01292414190464157182 ) ) ;
#21366 = VECTOR ( 'NONE', #21261, 1000.000000000000114 ) ;
#21367 = DIRECTION ( 'NONE',  ( 0.9770372205688160339, -0.2127605332646582970, -0.01145535281434409587 ) ) ;
#21368 = VERTEX_POINT ( 'NONE', #14754 ) ;
#21369 = CARTESIAN_POINT ( 'NONE',  ( 1.364373935098378649E-14, 105.0000000000000000, -9.836450281572198869E-15 ) ) ;
#21370 = ORIENTED_EDGE ( 'NONE', *, *, #1414, .T. ) ;
#21371 = DIRECTION ( 'NONE',  ( 0.1296504907605108559, 0.005475273188901296634, 0.9915446392518419971 ) ) ;
#21372 = CARTESIAN_POINT ( 'NONE',  ( 49.10244780775150275, 189.5926834231606506, -74.57745705999737140 ) ) ;
#21373 = CARTESIAN_POINT ( 'NONE',  ( -22.49358496127895535, 324.7653478115763050, 320.5678661935266973 ) ) ;
#21374 = PRODUCT_RELATED_PRODUCT_CATEGORY ( 'part', '', ( #9749 ) ) ;
#21375 = DIRECTION ( 'NONE',  ( 0.9232306267972774094, 0.000000000000000000, -0.3842462878721227826 ) ) ;
#21376 = ORIENTED_EDGE ( 'NONE', *, *, #16172, .T. ) ;
#21377 = CARTESIAN_POINT ( 'NONE',  ( -70.64248633631808616, 93.58690533528225330, 84.33313170347786070 ) ) ;
#21378 = CARTESIAN_POINT ( 'NONE',  ( -50.59410441606110709, 108.7350245882374224, -45.64162094458681196 ) ) ;
#21379 = VERTEX_POINT ( 'NONE', #18289 ) ;
#21380 = DIRECTION ( 'NONE',  ( -0.003413786507415475339, 0.9644842718275420390, -0.2641182225045781706 ) ) ;
#21381 = EDGE_LOOP ( 'NONE', ( #13729, #15490, #10892, #1401 ) ) ;
#21382 = CIRCLE ( 'NONE', #15545, 15.00000000000000533 ) ;
#21383 = VERTEX_POINT ( 'NONE', #21704 ) ;
#21384 = VERTEX_POINT ( 'NONE', #13029 ) ;
#21385 = AXIS2_PLACEMENT_3D ( 'NONE', #10013, #16802, #10234 ) ;
#21386 = CARTESIAN_POINT ( 'NONE',  ( -105.4334892372614121, 71.72994009789537984, 31.36525700924958926 ) ) ;
#21387 = CARTESIAN_POINT ( 'NONE',  ( 146.4999999999998579, 18.00000000000000355, -10.00000000000202860 ) ) ;
#21388 = EDGE_CURVE ( 'NONE', #8537, #21685, #21427, .T. ) ;
#21390 = ORIENTED_EDGE ( 'NONE', *, *, #21388, .F. ) ;
#21389 = VERTEX_POINT ( 'NONE', #18417 ) ;
#21391 = CARTESIAN_POINT ( 'NONE',  ( -49.61360656010212722, 118.9155345184949653, 166.8635573802473857 ) ) ;
#21392 = DIRECTION ( 'NONE',  ( 0.01292394549866728200, 0.005513023399720295634, 0.9999012842304692006 ) ) ;
#21393 = CARTESIAN_POINT ( 'NONE',  ( -1.761514441332976855, 142.7342175572188694, 274.9248293644216687 ) ) ;
#21394 = AXIS2_PLACEMENT_3D ( 'NONE', #17465, #13679, #11951 ) ;
#21395 = VECTOR ( 'NONE', #21071, 1000.000000000000227 ) ;
#21396 = CARTESIAN_POINT ( 'NONE',  ( -38.16379472481928303, 167.4246674330582891, 277.1335223284390850 ) ) ;
#21397 = PLANE ( 'NONE',  #8926 ) ;
#21398 = CARTESIAN_POINT ( 'NONE',  ( -56.08328763590613164, 143.6018742220275044, 109.9799478008652471 ) ) ;
#21399 = DIRECTION ( 'NONE',  ( -0.9999164797902015955, -6.965998958219364448E-18, 0.01292414190464157182 ) ) ;
#21400 = CARTESIAN_POINT ( 'NONE',  ( 16.16886689564234203, 187.9666359398803195, 308.7864178224293710 ) ) ;
#21401 = CIRCLE ( 'NONE', #11523, 3.399999999999991918 ) ;
#21402 = FACE_OUTER_BOUND ( 'NONE', #13686, .T. ) ;
#21403 = CIRCLE ( 'NONE', #14091, 126.0000000000000000 ) ;
#21404 = EDGE_CURVE ( 'NONE', #18381, #16056, #14985, .T. ) ;
#21405 = CARTESIAN_POINT ( 'NONE',  ( 55.40268456415108744, 20.00000000000000000, 113.1659955246503557 ) ) ;
#21406 = ORIENTED_EDGE ( 'NONE', *, *, #155, .T. ) ;
#21407 = EDGE_CURVE ( 'NONE', #6632, #8624, #9446, .T. ) ;
#21408 = CARTESIAN_POINT ( 'NONE',  ( -45.67464185259402853, 168.2105890667581605, -51.90496219196452188 ) ) ;
#21409 = CARTESIAN_POINT ( 'NONE',  ( -66.54881943730367766, 192.1904093341287307, 35.33996588919776372 ) ) ;
#21410 = VERTEX_POINT ( 'NONE', #735 ) ;
#21411 = CIRCLE ( 'NONE', #17408, 2.000000000000004885 ) ;
#21412 = CARTESIAN_POINT ( 'NONE',  ( -92.53737097235195108, 79.85828562204767422, -28.87839056718415875 ) ) ;
#21413 = ORIENTED_EDGE ( 'NONE', *, *, #17199, .F. ) ;
#21414 = ORIENTED_EDGE ( 'NONE', *, *, #3629, .F. ) ;
#21415 = VECTOR ( 'NONE', #18180, 1000.000000000000227 ) ;
#21416 = EDGE_CURVE ( 'NONE', #19195, #7339, #5538, .T. ) ;
#21417 = EDGE_CURVE ( 'NONE', #18898, #15229, #7732, .T. ) ;
#21418 = VECTOR ( 'NONE', #22568, 999.9999999999998863 ) ;
#21419 = DIRECTION ( 'NONE',  ( -0.01292394549866733230, -0.005513023399720419666, -0.9999012842304692006 ) ) ;
#21420 = ADVANCED_FACE ( 'NONE', ( #15660 ), #19840, .T. ) ;
#21421 = DIRECTION ( 'NONE',  ( -0.9232306267972777425, 0.000000000000000000, 0.3842462878721220054 ) ) ;
#21422 = CARTESIAN_POINT ( 'NONE',  ( -41.84548474893134085, 165.9069838518206836, 244.1862188963381755 ) ) ;
#21423 = DIRECTION ( 'NONE',  ( -0.01292394549866695240, -0.005513023399718316314, -0.9999012842304693116 ) ) ;
#21424 = CARTESIAN_POINT ( 'NONE',  ( 49.03340997568240311, 189.5897628274961164, -75.10636390159697839 ) ) ;
#21425 = CARTESIAN_POINT ( 'NONE',  ( -44.28529243912000624, 178.1224293456637042, 277.1536612075450421 ) ) ;
#21426 = ORIENTED_EDGE ( 'NONE', *, *, #3227, .F. ) ;
#21428 = CARTESIAN_POINT ( 'NONE',  ( -13.98112707844397562, 325.7531995422979207, 324.1294444254230598 ) ) ;
#21427 = B_SPLINE_CURVE_WITH_KNOTS ( 'NONE', 3,
 ( #19990, #2548, #9554, #11389, #951, #5888, #622, #21828, #4163, #20354, #13142, #14886, #2565, #11406 ),
 .UNSPECIFIED., .F., .F.,
 ( 4, 2, 2, 2, 2, 2, 4 ),
 ( -9.867989413304089735E-06, 0.0008231430655169662313, 0.001239648592982118581, 0.001656154120447271040, 0.002489165175377561212, 0.002905670702842706298, 0.003322176230307851384 ),
 .UNSPECIFIED. ) ;
#21429 = ORIENTED_EDGE ( 'NONE', *, *, #18247, .F. ) ;
#21430 = CIRCLE ( 'NONE', #5657, 3.099999999999998757 ) ;
#21431 = DIRECTION ( 'NONE',  ( -0.9770372205688159228, 0.2127605332646583802, 0.01145535281434409414 ) ) ;
#21432 = ADVANCED_FACE ( 'NONE', ( #17048 ), #8192, .T. ) ;
#21433 = CARTESIAN_POINT ( 'NONE',  ( 52.64951385222703095, 106.8152934070036224, 70.24943021328142834 ) ) ;
#21434 = CARTESIAN_POINT ( 'NONE',  ( -8.923556136456276988, 185.7170635346084850, 321.2501826865298540 ) ) ;
#21435 = CARTESIAN_POINT ( 'NONE',  ( -92.43457499998878291, 77.12912189496640281, 31.19724316448926871 ) ) ;
#21436 = CARTESIAN_POINT ( 'NONE',  ( -10.89406810251570867, 163.6808686305110143, 123.6704018889790717 ) ) ;
#21437 = ORIENTED_EDGE ( 'NONE', *, *, #7978, .T. ) ;
#21438 = CARTESIAN_POINT ( 'NONE',  ( -41.59208321381909457, 69.99999999999998579, -84.46951292587610283 ) ) ;
#21439 = AXIS2_PLACEMENT_3D ( 'NONE', #10269, #20820, #17284 ) ;
#21440 = ADVANCED_FACE ( 'NONE', ( #16929 ), #10139, .T. ) ;
#21441 = DIRECTION ( 'NONE',  ( -0.9999164797902015955, 0.000000000000000000, 0.01292414190464131335 ) ) ;
#21442 = CARTESIAN_POINT ( 'NONE',  ( -15.09688200079015985, 178.5583548832944416, 314.9430077195087847 ) ) ;
#21443 = ORIENTED_EDGE ( 'NONE', *, *, #21724, .T. ) ;
#21444 = ORIENTED_EDGE ( 'NONE', *, *, #11084, .F. ) ;
#21445 = LINE ( 'NONE', #5706, #8060 ) ;
#21446 =( BOUNDED_SURFACE ( )  B_SPLINE_SURFACE ( 1, 3, ( 
 ( #3244, #18878, #11893, #15683 ),
 ( #15349, #4736, #15575, #8217 ) ),
 .UNSPECIFIED., .F., .F., .T. ) 
 B_SPLINE_SURFACE_WITH_KNOTS ( ( 2, 2 ),
 ( 4, 4 ),
 ( 0.000000000000000000, 1.000000000000000000 ),
 ( 0.000000000000000000, 1.000000000000000000 ),
 .UNSPECIFIED. ) 
 GEOMETRIC_REPRESENTATION_ITEM ( )  RATIONAL_B_SPLINE_SURFACE ( (
 ( 1.000000000000000000, 0.9999999775413713765, 0.9999999775413713765, 1.000000000000000000),
 ( 1.000000000000000000, 0.9999999775413713765, 0.9999999775413713765, 1.000000000000000000) ) ) 
 REPRESENTATION_ITEM ( '' )  SURFACE ( )  );
#21447 = CIRCLE ( 'NONE', #16715, 2.000000000000001332 ) ;
#21448 = EDGE_LOOP ( 'NONE', ( #18416, #17756, #15980 ) ) ;
#21449 = CARTESIAN_POINT ( 'NONE',  ( 19.17021917716708046, 137.4993252555668164, 90.42132816724482325 ) ) ;
#21450 = EDGE_CURVE ( 'NONE', #8826, #12812, #4828, .T. ) ;
#21451 = CARTESIAN_POINT ( 'NONE',  ( -0.4135725409485391246, 69.99999999999998579, -31.99732735328654343 ) ) ;
#21452 = CARTESIAN_POINT ( 'NONE',  ( 49.42906846900682893, 109.0956092834914557, -47.06454438088354664 ) ) ;
#21453 = ORIENTED_EDGE ( 'NONE', *, *, #2550, .T. ) ;
#21454 = CARTESIAN_POINT ( 'NONE',  ( -45.96244189366829858, 171.4878726268958360, -74.17150848012535391 ) ) ;
#21455 = CARTESIAN_POINT ( 'NONE',  ( -53.12424548001075664, 118.8900173874207837, 162.2800983528087215 ) ) ;
#21456 = ORIENTED_EDGE ( 'NONE', *, *, #4275, .T. ) ;
#21457 = CARTESIAN_POINT ( 'NONE',  ( -4.656860399053663890, 189.4255402448441714, 275.7688761517259763 ) ) ;
#21458 = CARTESIAN_POINT ( 'NONE',  ( -49.99582398951010731, 170.0000000000000284, 0.6462070952320568828 ) ) ;
#21459 =( GEOMETRIC_REPRESENTATION_CONTEXT ( 3 ) GLOBAL_UNCERTAINTY_ASSIGNED_CONTEXT ( ( #272 ) ) GLOBAL_UNIT_ASSIGNED_CONTEXT ( ( #22042, #7838, #11392 ) ) REPRESENTATION_CONTEXT ( 'NONE', 'WORKASPACE' ) );
#21460 = CARTESIAN_POINT ( 'NONE',  ( -40.54224781076989359, 96.08381321950558629, -41.69419662078171029 ) ) ;
#21461 = CARTESIAN_POINT ( 'NONE',  ( -40.54264932485133954, 123.7663955596447352, -41.72526100787018777 ) ) ;
#21462 = ORIENTED_EDGE ( 'NONE', *, *, #11950, .T. ) ;
#21463 = ADVANCED_FACE ( 'NONE', ( #22604 ), #12085, .T. ) ;
#21464 = DIRECTION ( 'NONE',  ( -0.9999164797902015955, -6.965998958219364448E-18, 0.01292414190464157182 ) ) ;
#21465 = LINE ( 'NONE', #927, #19039 ) ;
#21466 = ORIENTED_EDGE ( 'NONE', *, *, #18655, .T. ) ;
#21467 = CARTESIAN_POINT ( 'NONE',  ( 41.91269397665269736, 107.0042359879021632, 70.57355413301411318 ) ) ;
#21468 = CARTESIAN_POINT ( 'NONE',  ( -88.17722787152888486, 89.00271273184408471, 51.54359545513624141 ) ) ;
#21469 = EDGE_CURVE ( 'NONE', #4209, #530, #6680, .T. ) ;
#21470 = CARTESIAN_POINT ( 'NONE',  ( -3.558528459570483360, 174.1198169369959317, 323.9878838343831262 ) ) ;
#21471 = CIRCLE ( 'NONE', #10114, 8.000000000000012434 ) ;
#21472 = ORIENTED_EDGE ( 'NONE', *, *, #3400, .T. ) ;
#21473 = ORIENTED_EDGE ( 'NONE', *, *, #1278, .F. ) ;
#21474 = DIRECTION ( 'NONE',  ( -0.7912924530843117310, 0.6113994113550571541, 0.006856638134102506846 ) ) ;
#21475 = CARTESIAN_POINT ( 'NONE',  ( 0.000000000000000000, 18.00000000000000355, 124.0000000000000000 ) ) ;
#21476 = DIRECTION ( 'NONE',  ( -0.01292394549866739822, -0.005513023399720312981, -0.9999012842304692006 ) ) ;
#21477 = CARTESIAN_POINT ( 'NONE',  ( -90.55526626895678532, 99.16641366430590665, -62.44901868852807070 ) ) ;
#21478 = ORIENTED_EDGE ( 'NONE', *, *, #18668, .F. ) ;
#21479 = CARTESIAN_POINT ( 'NONE',  ( 91.23603883849617091, 78.43035437438882695, 30.82342686631245243 ) ) ;
#21480 = ORIENTED_EDGE ( 'NONE', *, *, #17572, .F. ) ;
#21481 = FACE_OUTER_BOUND ( 'NONE', #16419, .T. ) ;
#21482 = DIRECTION ( 'NONE',  ( 0.1296504907605101897, 0.005475273188901851745, 0.9915446392518422192 ) ) ;
#21483 = DIRECTION ( 'NONE',  ( -0.000000000000000000, -1.000000000000000000, -0.000000000000000000 ) ) ;
#21484 = CARTESIAN_POINT ( 'NONE',  ( 0.000000000000000000, 20.00000000000000000, 0.000000000000000000 ) ) ;
#21485 = DIRECTION ( 'NONE',  ( -7.125109674025824596E-05, 0.9999848031710253382, -0.005512562950849464634 ) ) ;
#21486 = ORIENTED_EDGE ( 'NONE', *, *, #16005, .T. ) ;
#21487 = EDGE_CURVE ( 'NONE', #15318, #1967, #20617, .T. ) ;
#21488 = FACE_OUTER_BOUND ( 'NONE', #12551, .T. ) ;
#21489 = DIRECTION ( 'NONE',  ( 0.9999164797902015955, 6.965998958219364448E-18, -0.01292414190464157182 ) ) ;
#21490 = EDGE_CURVE ( 'NONE', #8785, #6866, #18390, .T. ) ;
#21491 = CARTESIAN_POINT ( 'NONE',  ( 40.83918162370624572, 106.3640148094703193, 92.25234674474768326 ) ) ;
#21492 = ORIENTED_EDGE ( 'NONE', *, *, #6692, .F. ) ;
#21493 = LINE ( 'NONE', #18294, #7997 ) ;
#21494 = ORIENTED_EDGE ( 'NONE', *, *, #21972, .F. ) ;
#21495 = ORIENTED_EDGE ( 'NONE', *, *, #5379, .F. ) ;
#21496 = CARTESIAN_POINT ( 'NONE',  ( -84.45439400451301992, 75.03386225069931470, -1.459998722890992529 ) ) ;
#21497 = CARTESIAN_POINT ( 'NONE',  ( -90.13473535659075253, 88.31972838967021744, 52.90262112213743251 ) ) ;
#21498 = ORIENTED_EDGE ( 'NONE', *, *, #9253, .T. ) ;
#21499 = CARTESIAN_POINT ( 'NONE',  ( 39.45107005634390873, 96.08378987033916019, -42.72816790301998680 ) ) ;
#21500 = CARTESIAN_POINT ( 'NONE',  ( -12.30122876842438373, 148.2386865495960251, 278.7941984645188427 ) ) ;
#21501 = DIRECTION ( 'NONE',  ( -0.01292394549866740169, -0.005513023399719847208, -0.9999012842304693116 ) ) ;
#21502 = CARTESIAN_POINT ( 'NONE',  ( -37.96378961924382622, 94.67635697584128707, 83.69533418420149928 ) ) ;
#21503 = PLANE ( 'NONE',  #7703 ) ;
#21504 = CARTESIAN_POINT ( 'NONE',  ( 18.61477174969464699, 185.5695927475049132, 278.0502835483144395 ) ) ;
#21505 = CARTESIAN_POINT ( 'NONE',  ( 16.47858955813311965, 187.6702387035254560, 308.9588621408448716 ) ) ;
#21506 = CARTESIAN_POINT ( 'NONE',  ( 3.596201236416850744, 188.2946505370595673, 294.4804741291034134 ) ) ;
#21507 = DIRECTION ( 'NONE',  ( -0.7056475024472774749, 0.7085438702141408918, 0.005214045635221195574 ) ) ;
#21508 = ORIENTED_EDGE ( 'NONE', *, *, #15159, .T. ) ;
#21509 = CARTESIAN_POINT ( 'NONE',  ( 45.23725195521918607, 161.1026720614313206, 18.06493089966673082 ) ) ;
#21510 = CARTESIAN_POINT ( 'NONE',  ( -55.33804461215960657, 114.2193244133317904, 167.6379947637574617 ) ) ;
#21511 = ORIENTED_EDGE ( 'NONE', *, *, #3564, .F. ) ;
#21512 = FACE_OUTER_BOUND ( 'NONE', #6166, .T. ) ;
#21513 = ORIENTED_EDGE ( 'NONE', *, *, #16967, .T. ) ;
#21514 = ORIENTED_EDGE ( 'NONE', *, *, #3040, .F. ) ;
#21515 = FACE_OUTER_BOUND ( 'NONE', #21801, .T. ) ;
#21516 = CARTESIAN_POINT ( 'NONE',  ( -2.180642712250698612, 70.14698466122827369, -99.20033613248658355 ) ) ;
#21517 = ADVANCED_FACE ( 'NONE', ( #8619 ), #15327, .F. ) ;
#21518 = CARTESIAN_POINT ( 'NONE',  ( -3.227672524189195702, 173.4898748461659750, 324.6532631065690566 ) ) ;
#21519 = CARTESIAN_POINT ( 'NONE',  ( 75.04638230800617293, 75.00896870829117802, -2.285242870542876670 ) ) ;
#21520 = CARTESIAN_POINT ( 'NONE',  ( -90.69261420090155923, 70.46556216177638987, 63.01891427407564095 ) ) ;
#21521 = CARTESIAN_POINT ( 'NONE',  ( -162.0000000000000000, 20.00000000000000000, 10.00000000000001954 ) ) ;
#21522 = DIRECTION ( 'NONE',  ( -7.125109674159588039E-05, 0.9999848031710253382, -0.005512562950848870491 ) ) ;
#21523 = CARTESIAN_POINT ( 'NONE',  ( 3.575103298931712636, 166.5249713112435188, 276.5989983650335375 ) ) ;
#21524 = ORIENTED_EDGE ( 'NONE', *, *, #21827, .F. ) ;
#21525 = DIRECTION ( 'NONE',  ( 5.440186201345738641E-18, 1.000000000000000000, 1.334940939666364181E-17 ) ) ;
#21526 = DIRECTION ( 'NONE',  ( 0.000000000000000000, 0.000000000000000000, 1.000000000000000000 ) ) ;
#21527 = DIRECTION ( 'NONE',  ( 0.8981428216242028917, 0.000000000000000000, 0.4397038457472429718 ) ) ;
#21528 = AXIS2_PLACEMENT_3D ( 'NONE', #21154, #9079, #17858 ) ;
#21529 = CARTESIAN_POINT ( 'NONE',  ( 52.26505271951528897, 106.8780608862217605, 70.19009726951736639 ) ) ;
#21530 = CARTESIAN_POINT ( 'NONE',  ( -45.67439959886510081, 164.8106407359766763, -51.88621947793163258 ) ) ;
#21531 = CARTESIAN_POINT ( 'NONE',  ( -90.73345939407629146, 80.10652859373118417, 31.90946778207756651 ) ) ;
#21532 = DIRECTION ( 'NONE',  ( -0.9999164797902015955, 0.000000000000000000, 0.01292414190464174703 ) ) ;
#21533 = ORIENTED_EDGE ( 'NONE', *, *, #11174, .T. ) ;
#21534 = EDGE_CURVE ( 'NONE', #13344, #14492, #20911, .T. ) ;
#21535 = CARTESIAN_POINT ( 'NONE',  ( -158.3970384574724619, 2.000000000000000000, -62.74304228515457993 ) ) ;
#21536 = EDGE_CURVE ( 'NONE', #11196, #7781, #11022, .T. ) ;
#21537 = CYLINDRICAL_SURFACE ( 'NONE', #15446, 2.000000000000004885 ) ;
#21538 = CARTESIAN_POINT ( 'NONE',  ( -15.10727221577994150, 179.7316785371915842, 313.5422839745355645 ) ) ;
#21539 = ORIENTED_EDGE ( 'NONE', *, *, #7731, .T. ) ;
#21540 = ORIENTED_EDGE ( 'NONE', *, *, #5822, .F. ) ;
#21541 = CARTESIAN_POINT ( 'NONE',  ( 51.02636103669043166, 169.5865232450209703, -75.66465169632658672 ) ) ;
#21542 = ORIENTED_EDGE ( 'NONE', *, *, #6717, .T. ) ;
#21543 = AXIS2_PLACEMENT_3D ( 'NONE', #20894, #15994, #22590 ) ;
#21544 = FACE_OUTER_BOUND ( 'NONE', #18036, .T. ) ;
#21545 = EDGE_CURVE ( 'NONE', #12590, #5759, #4436, .T. ) ;
#21546 = EDGE_CURVE ( 'NONE', #4404, #18312, #5634, .T. ) ;
#21547 = VERTEX_POINT ( 'NONE', #3569 ) ;
#21548 = CARTESIAN_POINT ( 'NONE',  ( -55.33804461215960657, 114.2193244133317904, 167.6379947637574617 ) ) ;
#21549 = ADVANCED_FACE ( 'NONE', ( #1975 ), #12768, .T. ) ;
#21550 = CARTESIAN_POINT ( 'NONE',  ( 50.50946076891578684, 111.5620289191883643, -47.97866760800079788 ) ) ;
#21551 = ORIENTED_EDGE ( 'NONE', *, *, #8103, .F. ) ;
#21552 = DIRECTION ( 'NONE',  ( 0.01292394549866737741, 0.005513023399721125699, 0.9999012842304693116 ) ) ;
#21553 = ORIENTED_EDGE ( 'NONE', *, *, #2239, .T. ) ;
#21554 = DIRECTION ( 'NONE',  ( 0.5617652846616786322, -0.7071067811865489050, 0.4294412240912380274 ) ) ;
#21555 = EDGE_LOOP ( 'NONE', ( #5345, #10466, #15376, #20898, #3691, #20009, #7411, #10048, #6255, #14070 ) ) ;
#21556 = PLANE ( 'NONE',  #3736 ) ;
#21557 = CARTESIAN_POINT ( 'NONE',  ( 12.49496009795829643, 188.8219583466606082, 321.3857951847916183 ) ) ;
#21558 = DIRECTION ( 'NONE',  ( 0.01292394549866731149, 0.005513023399720593139, 0.9999012842304692006 ) ) ;
#21559 = DIRECTION ( 'NONE',  ( 0.9506032891036972909, -0.3102281881984320644, -0.01057629388542894074 ) ) ;
#21560 = CIRCLE ( 'NONE', #15365, 5.999999999999952038 ) ;
#21561 = EDGE_CURVE ( 'NONE', #1423, #12640, #1743, .T. ) ;
#21562 = CARTESIAN_POINT ( 'NONE',  ( 2.830031787867828275, 70.80384757729338219, -80.39798906481894392 ) ) ;
#21563 = ADVANCED_FACE ( 'NONE', ( #8721 ), #12932, .T. ) ;
#21564 = EDGE_CURVE ( 'NONE', #7316, #4942, #14167, .T. ) ;
#21565 = LINE ( 'NONE', #5840, #17980 ) ;
#21566 = ORIENTED_EDGE ( 'NONE', *, *, #2832, .T. ) ;
#21567 = CARTESIAN_POINT ( 'NONE',  ( -88.17830160593697997, 89.00999716261956962, 51.42151637835925726 ) ) ;
#21568 = APPLICATION_PROTOCOL_DEFINITION ( 'draft international standard', 'automotive_design', 1998, #5421 ) ;
#21569 = VECTOR ( 'NONE', #9689, 1000.000000000000000 ) ;
#21571 = VERTEX_POINT ( 'NONE', #16238 ) ;
#21570 = ORIENTED_EDGE ( 'NONE', *, *, #4125, .F. ) ;
#21572 = FACE_OUTER_BOUND ( 'NONE', #4582, .T. ) ;
#21573 = EDGE_CURVE ( 'NONE', #6576, #10751, #3906, .T. ) ;
#21574 = EDGE_LOOP ( 'NONE', ( #21227, #7934 ) ) ;
#21575 = CARTESIAN_POINT ( 'NONE',  ( -41.44394036008644377, 166.0782723806960064, 275.2529508106263734 ) ) ;
#21576 = CARTESIAN_POINT ( 'NONE',  ( -49.99724901144494282, 189.9996960634205436, 0.5359558362150538269 ) ) ;
#21577 = CARTESIAN_POINT ( 'NONE',  ( 93.58499681124563097, 69.99999999999998579, 57.80872228166916926 ) ) ;
#21578 = CARTESIAN_POINT ( 'NONE',  ( -90.13422078941495386, 99.92632882282082107, -63.05520142610598811 ) ) ;
#21579 = ORIENTED_EDGE ( 'NONE', *, *, #2179, .T. ) ;
#21580 = CARTESIAN_POINT ( 'NONE',  ( 91.92156639752096225, 77.41735670888593290, 29.28407961425095962 ) ) ;
#21581 = ORIENTED_EDGE ( 'NONE', *, *, #12030, .T. ) ;
#21582 = DIRECTION ( 'NONE',  ( 0.01292394549866738782, 0.005513023399720468239, 0.9999012842304692006 ) ) ;
#21583 = CARTESIAN_POINT ( 'NONE',  ( 49.03514658276407800, 189.5905036194994864, -74.97200588752639305 ) ) ;
#21584 = DIRECTION ( 'NONE',  ( 0.1296504907605108559, 0.005475273188901296634, 0.9915446392518419971 ) ) ;
#21585 = CARTESIAN_POINT ( 'NONE',  ( -22.61872943466546104, 324.6985644157359729, 307.5651070260664142 ) ) ;
#21586 = AXIS2_PLACEMENT_3D ( 'NONE', #19564, #14082, #5319 ) ;
#21587 = CARTESIAN_POINT ( 'NONE',  ( 19.42556530730579567, 136.7551719540686008, -44.57217540897067920 ) ) ;
#21588 = ADVANCED_FACE ( 'NONE', ( #9186 ), #7478, .F. ) ;
#21589 = ORIENTED_EDGE ( 'NONE', *, *, #14157, .T. ) ;
#21590 = CARTESIAN_POINT ( 'NONE',  ( -91.62437796271721879, 72.00000000000000000, -60.86849236629028326 ) ) ;
#21591 = CARTESIAN_POINT ( 'NONE',  ( -9.472248412593195610, 81.99999999999998579, -86.53426659026914081 ) ) ;
#21592 = VECTOR ( 'NONE', #8467, 1000.000000000000114 ) ;
#21593 = CARTESIAN_POINT ( 'NONE',  ( -51.40218462123966248, 189.4003865961453812, -108.1612621023553658 ) ) ;
#21594 = EDGE_LOOP ( 'NONE', ( #15434, #7798, #9072, #13385 ) ) ;
#21595 = LINE ( 'NONE', #19883, #18272 ) ;
#21596 = CARTESIAN_POINT ( 'NONE',  ( 51.99565694909048830, 170.0000000000000284, -0.6720553790413839046 ) ) ;
#21597 = ORIENTED_EDGE ( 'NONE', *, *, #4872, .T. ) ;
#21598 = CARTESIAN_POINT ( 'NONE',  ( -81.25051790709260047, 75.12836414114961769, 5.987897703801240645 ) ) ;
#21599 = CARTESIAN_POINT ( 'NONE',  ( -90.16949869353247493, 87.13201789581339085, 51.31799079330890123 ) ) ;
#21600 = AXIS2_PLACEMENT_3D ( 'NONE', #17738, #19867, #19423 ) ;
#21601 = VERTEX_POINT ( 'NONE', #17603 ) ;
#21602 = CIRCLE ( 'NONE', #9153, 2.499999999999988010 ) ;
#21603 = EDGE_CURVE ( 'NONE', #21849, #19075, #7780, .T. ) ;
#21604 = EDGE_CURVE ( 'NONE', #11013, #5296, #5511, .T. ) ;
#21605 = CONICAL_SURFACE ( 'NONE', #7322, 5.700000000000003730, 0.7853981633974482790 ) ;
#21606 = CARTESIAN_POINT ( 'NONE',  ( -90.40889375659909888, 72.00000000000000000, 33.17122784026039284 ) ) ;
#21607 = DIRECTION ( 'NONE',  ( -2.025474946048326158E-22, 1.000000000000000000, -1.876735158486678933E-22 ) ) ;
#21608 = FACE_OUTER_BOUND ( 'NONE', #15956, .T. ) ;
#21609 = CARTESIAN_POINT ( 'NONE',  ( -37.84108139470004772, 94.62834100696746020, 83.74230054658565336 ) ) ;
#21610 = CARTESIAN_POINT ( 'NONE',  ( 9.196690372329049623, 142.8086146031528187, 274.7267082784170498 ) ) ;
#21611 = CARTESIAN_POINT ( 'NONE',  ( 74.35083714549891454, 75.04017415462969609, -3.729659851975327900 ) ) ;
#21612 = CARTESIAN_POINT ( 'NONE',  ( 19.24716218600273976, 184.5819132463487904, 316.9868485712452184 ) ) ;
#21613 = CARTESIAN_POINT ( 'NONE',  ( 69.43142427201327394, 92.58578643762697880, -85.31868097644085935 ) ) ;
#21614 = AXIS2_PLACEMENT_3D ( 'NONE', #10768, #19594, #311 ) ;
#21615 = PRODUCT_DEFINITION_SHAPE ( 'NONE', 'NONE',  #20389 ) ;
#21616 = CIRCLE ( 'NONE', #13586, 112.5000000000000142 ) ;
#21617 = CARTESIAN_POINT ( 'NONE',  ( -53.01407513488474876, 118.5884715842524457, 107.5779438241560655 ) ) ;
#21618 = DIRECTION ( 'NONE',  ( 0.9232306267972774094, 0.000000000000000000, -0.3842462878721227826 ) ) ;
#21619 = ORIENTED_EDGE ( 'NONE', *, *, #2050, .T. ) ;
#21620 = SPHERICAL_SURFACE ( 'NONE', #12052, 2.000000000000000000 ) ;
#21621 = VERTEX_POINT ( 'NONE', #1852 ) ;
#21622 = ORIENTED_EDGE ( 'NONE', *, *, #11332, .F. ) ;
#21623 = CARTESIAN_POINT ( 'NONE',  ( -79.99331838321612054, 54.99999999999999289, 1.033931352371344481 ) ) ;
#21624 = CARTESIAN_POINT ( 'NONE',  ( -28.13117687807453038, -5.346239964818102486, -9.967962068994514979 ) ) ;
#21625 = AXIS2_PLACEMENT_3D ( 'NONE', #320, #3763, #9027 ) ;
#21626 = CARTESIAN_POINT ( 'NONE',  ( -2.067862704742604141, 72.00000000000000000, -159.9866367664322979 ) ) ;
#21627 = CARTESIAN_POINT ( 'NONE',  ( -88.72304114575449319, 70.71205020914676709, 62.85437454899338405 ) ) ;
#21628 = AXIS2_PLACEMENT_3D ( 'NONE', #2699, #5773, #977 ) ;
#21629 = DIRECTION ( 'NONE',  ( 0.000000000000000000, -1.000000000000000000, 0.000000000000000000 ) ) ;
#21630 = CARTESIAN_POINT ( 'NONE',  ( 74.24069787013584687, 75.02961117147833647, 1.434652486052601983 ) ) ;
#21631 = AXIS2_PLACEMENT_3D ( 'NONE', #16175, #9362, #415 ) ;
#21632 = DIRECTION ( 'NONE',  ( 0.6113012557851978945, 0.7913029548584308293, -0.01226410648014603956 ) ) ;
#21633 = AXIS2_PLACEMENT_3D ( 'NONE', #19546, #19869, #5866 ) ;
#21634 = ORIENTED_EDGE ( 'NONE', *, *, #20789, .F. ) ;
#21635 = DIRECTION ( 'NONE',  ( 0.01292414190464131508, 0.000000000000000000, 0.9999164797902017066 ) ) ;
#21636 = DIRECTION ( 'NONE',  ( 0.9701786850993898703, 0.001334069994602712916, 0.2423871680515871929 ) ) ;
#21637 = AXIS2_PLACEMENT_3D ( 'NONE', #6805, #12105, #13830 ) ;
#21638 = LINE ( 'NONE', #6396, #15234 ) ;
#21639 = CARTESIAN_POINT ( 'NONE',  ( -9.007069321288007302, 140.4227465520236251, 76.88579701175710568 ) ) ;
#21640 = CYLINDRICAL_SURFACE ( 'NONE', #5945, 101.0000000000000000 ) ;
#21641 = CARTESIAN_POINT ( 'NONE',  ( -89.23446290093953337, 79.53212074382820163, 30.14913290299145388 ) ) ;
#21642 = CARTESIAN_POINT ( 'NONE',  ( 39.18815798788130422, 105.5072037373731888, 91.67997329703011644 ) ) ;
#21643 = ORIENTED_EDGE ( 'NONE', *, *, #4704, .F. ) ;
#21644 = DIRECTION ( 'NONE',  ( 7.125109674403277385E-05, -0.9999848031710253382, 0.005512562950848281552 ) ) ;
#21645 = VERTEX_POINT ( 'NONE', #12544 ) ;
#21646 = DIRECTION ( 'NONE',  ( 0.9999164797902015955, -8.863511990578706951E-16, -0.01292414190464158050 ) ) ;
#21647 = CARTESIAN_POINT ( 'NONE',  ( -14.52510427035945995, 181.2105282831826116, 311.5198460221306505 ) ) ;
#21648 = VERTEX_POINT ( 'NONE', #19537 ) ;
#21649 = AXIS2_PLACEMENT_3D ( 'NONE', #10541, #6853, #22456 ) ;
#21650 = VERTEX_POINT ( 'NONE', #19638 ) ;
#21651 = CIRCLE ( 'NONE', #8823, 6.500000000000000000 ) ;
#21652 = CARTESIAN_POINT ( 'NONE',  ( -164.0000000000000000, 1.999999999999998224, -7.999999999999979572 ) ) ;
#21653 = CARTESIAN_POINT ( 'NONE',  ( 79.90518398323666815, 100.1635695855008095, 75.81005614957788907 ) ) ;
#21654 = AXIS2_PLACEMENT_3D ( 'NONE', #12966, #13396, #18137 ) ;
#21655 = ITEM_DEFINED_TRANSFORMATION ( 'NONE', 'NONE', #2945,  #6292 ) ;
#21656 = ADVANCED_FACE ( 'NONE', ( #19414 ), #16118, .T. ) ;
#21657 = EDGE_LOOP ( 'NONE', ( #5312, #7343, #10530, #20212 ) ) ;
#21658 = LINE ( 'NONE', #11349, #18093 ) ;
#21659 = EDGE_CURVE ( 'NONE', #11858, #1423, #5735, .T. ) ;
#21660 = CARTESIAN_POINT ( 'NONE',  ( -1.109343863968193944E-13, 20.00000000000000000, -7.999999999999994671 ) ) ;
#21661 = ORIENTED_EDGE ( 'NONE', *, *, #1489, .F. ) ;
#21662 = CARTESIAN_POINT ( 'NONE',  ( -11.46885069223597853, 81.19615242270661781, -91.33151364841882014 ) ) ;
#21663 = CARTESIAN_POINT ( 'NONE',  ( -14.86391513884368187, 178.8380028225893170, 318.6775144440179020 ) ) ;
#21664 = ORIENTED_EDGE ( 'NONE', *, *, #8921, .T. ) ;
#21665 = CARTESIAN_POINT ( 'NONE',  ( 12.62171595694235471, 189.1959137912106712, 321.1530085673936696 ) ) ;
#21666 = CIRCLE ( 'NONE', #5166, 2.000000000000004441 ) ;
#21667 = LINE ( 'NONE', #461, #17181 ) ;
#21668 = CARTESIAN_POINT ( 'NONE',  ( -46.67642080778155389, 127.4153035195788846, 257.4621697307391059 ) ) ;
#21669 = ORIENTED_EDGE ( 'NONE', *, *, #1542, .T. ) ;
#21670 = EDGE_CURVE ( 'NONE', #13772, #18610, #1188, .T. ) ;
#21671 = CARTESIAN_POINT ( 'NONE',  ( -6.892589744943404817, 164.5414928385482654, 81.72598018271095555 ) ) ;
#21672 = AXIS2_PLACEMENT_3D ( 'NONE', #9741, #11337, #13084 ) ;
#21673 = EDGE_CURVE ( 'NONE', #3218, #19636, #7350, .T. ) ;
#21674 = CARTESIAN_POINT ( 'NONE',  ( 58.87600894486503478, 126.5883500096209815, 106.0876318414197499 ) ) ;
#21675 = EDGE_CURVE ( 'NONE', #19859, #7803, #2184, .T. ) ;
#21676 = EDGE_LOOP ( 'NONE', ( #4203, #21298, #18500, #7566 ) ) ;
#21677 = UNCERTAINTY_MEASURE_WITH_UNIT (LENGTH_MEASURE( 1.000000000000000082E-05 ), #19171, 'distance_accuracy_value', 'NONE');
#21678 = CIRCLE ( 'NONE', #16960, 7.000000000000021316 ) ;
#21679 = CARTESIAN_POINT ( 'NONE',  ( -55.33837949231439524, 118.9192529882355984, 167.6120857178885899 ) ) ;
#21680 = VECTOR ( 'NONE', #20179, 1000.000000000000114 ) ;
#21681 = PLANE ( 'NONE',  #12297 ) ;
#21682 = DIRECTION ( 'NONE',  ( 1.000000000000000000, 0.000000000000000000, 0.000000000000000000 ) ) ;
#21683 = VECTOR ( 'NONE', #17848, 1000.000000000000000 ) ;
#21684 = EDGE_CURVE ( 'NONE', #16738, #15010, #9626, .T. ) ;
#21686 = VERTEX_POINT ( 'NONE', #4128 ) ;
#21685 = VERTEX_POINT ( 'NONE', #17727 ) ;
#21687 = ADVANCED_FACE ( 'NONE', ( #2310 ), #22025, .T. ) ;
#21688 = FACE_OUTER_BOUND ( 'NONE', #636, .T. ) ;
#21689 = EDGE_CURVE ( 'NONE', #17055, #2643, #22412, .T. ) ;
#21690 = CARTESIAN_POINT ( 'NONE',  ( -51.62794139783391500, 111.4615474418020682, -46.62154578428164342 ) ) ;
#21691 = EDGE_LOOP ( 'NONE', ( #19769, #4467, #19819, #15002 ) ) ;
#21692 = PLANE ( 'NONE',  #1911 ) ;
#21693 = CIRCLE ( 'NONE', #7416, 75.00000000000002842 ) ;
#21694 = CARTESIAN_POINT ( 'NONE',  ( 1.828589379190189046, 190.7803332315567388, 141.4745109201486457 ) ) ;
#21695 = EDGE_CURVE ( 'NONE', #8236, #15824, #13660, .T. ) ;
#21696 = DIRECTION ( 'NONE',  ( 0.2129978593076544968, 0.9766860055760742121, 0.02676487328961881657 ) ) ;
#21697 = CARTESIAN_POINT ( 'NONE',  ( 89.66113247980437961, 100.6041916471017856, 63.72504470331089266 ) ) ;
#21698 = CARTESIAN_POINT ( 'NONE',  ( -89.90836385050330648, 100.2819950034555205, -63.37719018575656094 ) ) ;
#21699 = VERTEX_POINT ( 'NONE', #2429 ) ;
#21700 = ORIENTED_EDGE ( 'NONE', *, *, #22220, .T. ) ;
#21701 = DIRECTION ( 'NONE',  ( 0.9232306267972777425, 0.000000000000000000, -0.3842462878721220054 ) ) ;
#21702 = CARTESIAN_POINT ( 'NONE',  ( 161.9999999999992610, 1.999999999999998224, 53.76161406891478123 ) ) ;
#21703 = LINE ( 'NONE', #5990, #22609 ) ;
#21704 = CARTESIAN_POINT ( 'NONE',  ( 146.4999999999998863, 18.00000000000000355, -8.000000000002026823 ) ) ;
#21705 = EDGE_CURVE ( 'NONE', #19445, #16346, #6675, .T. ) ;
#21706 = CARTESIAN_POINT ( 'NONE',  ( -51.36859115140752152, 114.2028473779704143, 164.5977368973751993 ) ) ;
#21707 = ORIENTED_EDGE ( 'NONE', *, *, #5822, .T. ) ;
#21708 = PLANE ( 'NONE',  #15534 ) ;
#21709 =( NAMED_UNIT ( * ) SI_UNIT ( $, .STERADIAN. ) SOLID_ANGLE_UNIT ( ) );
#21710 = ORIENTED_EDGE ( 'NONE', *, *, #12469, .T. ) ;
#21711 = DIRECTION ( 'NONE',  ( 0.9232306267972777425, 0.000000000000000000, -0.3842462878721220054 ) ) ;
#21712 = B_SPLINE_CURVE_WITH_KNOTS ( 'NONE', 3,
 ( #6828, #8653, #4982, #15480, #17180, #11909, #22433, #6503, #13956, #18891, #15696, #20492, #13746, #5212, #3155, #13847 ),
 .UNSPECIFIED., .F., .F.,
 ( 4, 2, 2, 2, 2, 2, 2, 4 ),
 ( 0.000000000000000000, 0.0003976901483970908080, 0.0007953802967941816160, 0.001193070445191272370, 0.001590760593588363232, 0.001988450741985454094, 0.002386140890382544739, 0.003181521187176709550 ),
 .UNSPECIFIED. ) ;
#21713 = EDGE_CURVE ( 'NONE', #6385, #3811, #20202, .T. ) ;
#21714 = CONICAL_SURFACE ( 'NONE', #3764, 3.047499999999988329, 1.047197551196594523 ) ;
#21715 = ORIENTED_EDGE ( 'NONE', *, *, #22408, .F. ) ;
#21716 = AXIS2_PLACEMENT_3D ( 'NONE', #13786, #15631, #19387 ) ;
#21717 = ORIENTED_EDGE ( 'NONE', *, *, #14013, .F. ) ;
#21718 = CARTESIAN_POINT ( 'NONE',  ( -79.92740525950245001, 75.13699351169597662, 6.133505399301365735 ) ) ;
#21719 =( REPRESENTATION_RELATIONSHIP ('NONE','NONE', #11808, #19567 ) REPRESENTATION_RELATIONSHIP_WITH_TRANSFORMATION ( #7446 )SHAPE_REPRESENTATION_RELATIONSHIP( ) );
#21720 = CARTESIAN_POINT ( 'NONE',  ( 13.03243690953249612, 190.3745391624070180, 307.8621314096817514 ) ) ;
#21721 = VECTOR ( 'NONE', #19948, 1000.000000000000114 ) ;
#21722 = ORIENTED_EDGE ( 'NONE', *, *, #10272, .T. ) ;
#21723 = AXIS2_PLACEMENT_3D ( 'NONE', #897, #2725, #8115 ) ;
#21724 = EDGE_CURVE ( 'NONE', #22024, #638, #4011, .T. ) ;
#21725 = CYLINDRICAL_SURFACE ( 'NONE', #6330, 4.199999999999997513 ) ;
#21726 = CARTESIAN_POINT ( 'NONE',  ( -9.732840034447848510, 187.7216402471333083, 276.1639041411631865 ) ) ;
#21727 = DIRECTION ( 'NONE',  ( 0.9934404589540163366, 0.1135548637187051429, -0.01346653032743023309 ) ) ;
#21728 = DIRECTION ( 'NONE',  ( -0.9934404589540163366, -0.1135548637187051429, 0.01346653032743023309 ) ) ;
#21729 = DIRECTION ( 'NONE',  ( -1.000000000000000000, 0.000000000000000000, -1.387778780781445833E-14 ) ) ;
#21730 = CARTESIAN_POINT ( 'NONE',  ( 15.82374578500689211, 187.4932621794992258, 277.2901064574259067 ) ) ;
#21731 = CARTESIAN_POINT ( 'NONE',  ( 19.94166477935907622, 183.4991379525720276, 314.2419295910784172 ) ) ;
#21732 = CARTESIAN_POINT ( 'NONE',  ( 146.4999999999998863, 1.999999999999998224, 8.000000000001989520 ) ) ;
#21733 = VECTOR ( 'NONE', #9252, 1000.000000000000114 ) ;
#21734 = AXIS2_PLACEMENT_3D ( 'NONE', #14335, #16180, #22657 ) ;
#21735 = EDGE_CURVE ( 'NONE', #10387, #12053, #9537, .T. ) ;
#21736 = DIRECTION ( 'NONE',  ( -0.000000000000000000, -1.000000000000000000, -0.000000000000000000 ) ) ;
#21737 = CARTESIAN_POINT ( 'NONE',  ( -11.23675596313486125, 155.5381941787832716, 97.81558748025744876 ) ) ;
#21738 = EDGE_LOOP ( 'NONE', ( #7591, #11162, #17510, #18060 ) ) ;
#21739 = CARTESIAN_POINT ( 'NONE',  ( 37.51330139321492396, 69.99999999999998579, -87.03232607370792095 ) ) ;
#21740 = VERTEX_POINT ( 'NONE', #9417 ) ;
#21741 = CARTESIAN_POINT ( 'NONE',  ( 47.42520555988353692, 108.9831309495507838, -44.78095393139386005 ) ) ;
#21742 = LINE ( 'NONE', #2588, #4559 ) ;
#21743 = AXIS2_PLACEMENT_3D ( 'NONE', #22534, #6502, #18785 ) ;
#21744 = CARTESIAN_POINT ( 'NONE',  ( 79.72645225953733927, 75.13699351169597662, 4.069943940015851247 ) ) ;
#21745 = CARTESIAN_POINT ( 'NONE',  ( -0.003538370294055813436, 69.99999999999998579, -98.91746206376724615 ) ) ;
#21746 = AXIS2_PLACEMENT_3D ( 'NONE', #6475, #22504, #20462 ) ;
#21747 = AXIS2_PLACEMENT_3D ( 'NONE', #14889, #7856, #13049 ) ;
#21748 = PLANE ( 'NONE',  #12997 ) ;
#21749 = DIRECTION ( 'NONE',  ( -5.440186201345738641E-18, -1.000000000000000000, -1.334940939666364181E-17 ) ) ;
#21750 = ORIENTED_EDGE ( 'NONE', *, *, #13731, .F. ) ;
#21751 = LINE ( 'NONE', #11561, #3997 ) ;
#21752 = CARTESIAN_POINT ( 'NONE',  ( 153.3508620259912618, -0.2263999372173197688, -43.05128410831431296 ) ) ;
#21753 = CARTESIAN_POINT ( 'NONE',  ( 89.63665673671270895, 97.44507682733028275, -63.75962087488073848 ) ) ;
#21754 = CARTESIAN_POINT ( 'NONE',  ( -39.32379867999515710, 107.5575245709147225, 72.11031038871728072 ) ) ;
#21755 = CARTESIAN_POINT ( 'NONE',  ( 68.68766895589033084, 71.65104882840748246, -85.91861595181279654 ) ) ;
#21756 = CARTESIAN_POINT ( 'NONE',  ( 91.65210746689167820, 71.62127171602892872, 60.82679172889523045 ) ) ;
#21757 = VECTOR ( 'NONE', #4509, 1000.000000000000227 ) ;
#21758 = AXIS2_PLACEMENT_3D ( 'NONE', #3548, #10343, #8599 ) ;
#21759 = ORIENTED_EDGE ( 'NONE', *, *, #880, .F. ) ;
#21760 = CARTESIAN_POINT ( 'NONE',  ( 49.28843399868946307, 189.4915746906123957, -92.92109297631797915 ) ) ;
#21761 = ADVANCED_FACE ( 'NONE', ( #18277 ), #2273, .T. ) ;
#21762 = PLANE ( 'NONE',  #2218 ) ;
#21763 = CARTESIAN_POINT ( 'NONE',  ( -14.18812936803128189, 179.9703185431055203, 311.0925469625015012 ) ) ;
#21764 = EDGE_CURVE ( 'NONE', #4883, #10934, #10340, .T. ) ;
#21765 = ORIENTED_EDGE ( 'NONE', *, *, #18737, .F. ) ;
#21766 = VECTOR ( 'NONE', #546, 999.9999999999998863 ) ;
#21767 = ORIENTED_EDGE ( 'NONE', *, *, #14311, .T. ) ;
#21768 = VECTOR ( 'NONE', #773, 999.9999999999998863 ) ;
#21769 = CARTESIAN_POINT ( 'NONE',  ( 0.002351286192456229947, 137.0005014953561897, 0.1819145773780327657 ) ) ;
#21770 = CARTESIAN_POINT ( 'NONE',  ( 11.89239805793121363, 187.8969028425499914, 305.8235062411625904 ) ) ;
#21771 = VECTOR ( 'NONE', #22004, 1000.000000000000114 ) ;
#21772 = ORIENTED_EDGE ( 'NONE', *, *, #21935, .F. ) ;
#21773 = PRODUCT_DEFINITION ( 'UNKNOWN', '', #8807, #22549 ) ;
#21774 = DIRECTION ( 'NONE',  ( 0.01292394549866731843, 0.005513023399720594006, 0.9999012842304693116 ) ) ;
#21775 = DIRECTION ( 'NONE',  ( 7.125109674364534776E-05, -0.9999848031710252272, 0.005512562950849704893 ) ) ;
#21776 = ORIENTED_EDGE ( 'NONE', *, *, #15275, .T. ) ;
#21777 = AXIS2_PLACEMENT_3D ( 'NONE', #21506, #3845, #10618 ) ;
#21778 = ORIENTED_EDGE ( 'NONE', *, *, #1349, .T. ) ;
#21779 = CIRCLE ( 'NONE', #9724, 2.000000000000004441 ) ;
#21780 = LINE ( 'NONE', #6067, #5380 ) ;
#21781 = CARTESIAN_POINT ( 'NONE',  ( -10.62552804867366518, 183.8325962315270203, 305.7046552162815942 ) ) ;
#21782 = ORIENTED_EDGE ( 'NONE', *, *, #17667, .T. ) ;
#21783 = CARTESIAN_POINT ( 'NONE',  ( -38.56600193350200811, 165.4640537929580830, 244.1462729796548103 ) ) ;
#21784 = CARTESIAN_POINT ( 'NONE',  ( -42.56628114047011735, 94.99786382055523859, -43.54068532293076288 ) ) ;
#21785 = CARTESIAN_POINT ( 'NONE',  ( -0.5690403138955768547, 86.15674685880075856, 75.02401767694439627 ) ) ;
#21786 = ADVANCED_FACE ( 'NONE', ( #4351 ), #11267, .T. ) ;
#21787 = ORIENTED_EDGE ( 'NONE', *, *, #12940, .F. ) ;
#21788 = DIRECTION ( 'NONE',  ( 7.125109674141484573E-05, -0.9999848031710252272, 0.005512562950851785694 ) ) ;
#21789 = ADVANCED_FACE ( 'NONE', ( #6089 ), #21692, .T. ) ;
#21790 = CARTESIAN_POINT ( 'NONE',  ( -8.773265341766837366, 185.9468773097319172, 306.9487736168949823 ) ) ;
#21791 = ORIENTED_EDGE ( 'NONE', *, *, #16578, .T. ) ;
#21792 = DIRECTION ( 'NONE',  ( 0.01292394549866738782, 0.005513023399720700692, 0.9999012842304693116 ) ) ;
#21793 = CARTESIAN_POINT ( 'NONE',  ( -88.90404157702997168, 89.05586475019977399, 50.97367400307179963 ) ) ;
#21794 = CARTESIAN_POINT ( 'NONE',  ( 116.6746474996916589, 14.99999999999998579, 81.15171273617272618 ) ) ;
#21795 = ORIENTED_EDGE ( 'NONE', *, *, #10299, .F. ) ;
#21796 = ADVANCED_FACE ( 'NONE', ( #16457 ), #13116, .T. ) ;
#21797 = CARTESIAN_POINT ( 'NONE',  ( 90.85853474116410666, 77.59429383720569717, -31.92673238494557353 ) ) ;
#21798 = EDGE_LOOP ( 'NONE', ( #3717, #9685, #21282, #19659 ) ) ;
#21799 = CARTESIAN_POINT ( 'NONE',  ( -9.912705577010314703E-16, 18.00000000000000355, -9.999999999999994671 ) ) ;
#21800 = FACE_OUTER_BOUND ( 'NONE', #18880, .T. ) ;
#21801 = EDGE_LOOP ( 'NONE', ( #11145, #11442, #274, #14696 ) ) ;
#21802 = AXIS2_PLACEMENT_3D ( 'NONE', #2171, #21464, #5724 ) ;
#21803 = FACE_OUTER_BOUND ( 'NONE', #13814, .T. ) ;
#21804 = DIRECTION ( 'NONE',  ( 0.1296504907605110779, 0.005475273188902231650, 0.9915446392518419971 ) ) ;
#21805 = EDGE_LOOP ( 'NONE', ( #8840, #19168, #13890, #18201 ) ) ;
#21806 = VERTEX_POINT ( 'NONE', #1037 ) ;
#21807 = FACE_OUTER_BOUND ( 'NONE', #1329, .T. ) ;
#21808 = CARTESIAN_POINT ( 'NONE',  ( -0.003538370294055813436, 81.99999999999998579, -98.91746206376724615 ) ) ;
#21809 = FACE_OUTER_BOUND ( 'NONE', #11779, .T. ) ;
#21810 = CARTESIAN_POINT ( 'NONE',  ( -56.92334409331949274, 143.2435277010456787, 44.98636432588479295 ) ) ;
#21811 = VERTEX_POINT ( 'NONE', #19860 ) ;
#21812 = DIRECTION ( 'NONE',  ( -1.000000000000000000, 0.000000000000000000, 1.386679829960243376E-14 ) ) ;
#21813 = DIRECTION ( 'NONE',  ( -0.9999164797902015955, -2.001050586450180341E-22, 0.01292414190464038874 ) ) ;
#21814 = CARTESIAN_POINT ( 'NONE',  ( -52.41270905777618339, 111.9218655255082524, -46.78102551800296283 ) ) ;
#21815 = ADVANCED_FACE ( 'NONE', ( #826, #16789 ), #11377, .T. ) ;
#21816 = ORIENTED_EDGE ( 'NONE', *, *, #15289, .T. ) ;
#21817 = CYLINDRICAL_SURFACE ( 'NONE', #19714, 2.000000000000001776 ) ;
#21818 = EDGE_CURVE ( 'NONE', #13676, #22322, #2656, .T. ) ;
#21819 = ORIENTED_EDGE ( 'NONE', *, *, #6613, .F. ) ;
#21820 = CIRCLE ( 'NONE', #11955, 10.00000000000001599 ) ;
#21821 = ORIENTED_EDGE ( 'NONE', *, *, #19870, .F. ) ;
#21822 = ORIENTED_EDGE ( 'NONE', *, *, #2689, .T. ) ;
#21823 = CARTESIAN_POINT ( 'NONE',  ( -82.48914589713568546, 75.10304909037272125, 5.494148405572993887 ) ) ;
#21824 = CARTESIAN_POINT ( 'NONE',  ( -90.17266153500538906, 87.07308075466939101, 51.35371910215589253 ) ) ;
#21825 = CARTESIAN_POINT ( 'NONE',  ( -42.64951291394369548, 126.1473081376431367, 27.39440536439884255 ) ) ;
#21826 = ORIENTED_EDGE ( 'NONE', *, *, #16705, .F. ) ;
#21827 = EDGE_CURVE ( 'NONE', #5334, #13470, #5188, .T. ) ;
#21828 = CARTESIAN_POINT ( 'NONE',  ( -38.08586061832574643, 105.9452655173670905, 92.44882592006047162 ) ) ;
#21829 = CARTESIAN_POINT ( 'NONE',  ( -10.85567112094788200, 105.6999953372425409, 127.2994028633183063 ) ) ;
#21830 = DIRECTION ( 'NONE',  ( 0.01292394549866733230, 0.005513023399720419666, 0.9999012842304692006 ) ) ;
#21831 = CARTESIAN_POINT ( 'NONE',  ( -39.10370113527942237, 92.00280690324824207, -83.45957852173413016 ) ) ;
#21832 = CARTESIAN_POINT ( 'NONE',  ( 53.31422965588423324, 141.4150907639734953, 256.0925796589630181 ) ) ;
#21833 = EDGE_CURVE ( 'NONE', #5334, #19478, #8033, .T. ) ;
#21834 = EDGE_LOOP ( 'NONE', ( #13399, #3474, #13615, #933 ) ) ;
#21835 = CARTESIAN_POINT ( 'NONE',  ( -44.20351303877662019, 168.2403975157799607, 277.2070894419563274 ) ) ;
#21836 = AXIS2_PLACEMENT_3D ( 'NONE', #13683, #5370, #5259 ) ;
#21837 = CARTESIAN_POINT ( 'NONE',  ( 73.77409342887030164, 75.00271445951732119, -1.775928710569730340 ) ) ;
#21838 = CARTESIAN_POINT ( 'NONE',  ( 18.26914968921775539, 184.2849635139225484, 318.6958977197980971 ) ) ;
#21839 = CARTESIAN_POINT ( 'NONE',  ( 23.05638568958544710, 89.37982582623894245, -78.77076284602109979 ) ) ;
#21840 = CARTESIAN_POINT ( 'NONE',  ( -65.93019277160487945, 189.6011917897851333, -71.54720792259536211 ) ) ;
#21841 =( NAMED_UNIT ( * ) SI_UNIT ( $, .STERADIAN. ) SOLID_ANGLE_UNIT ( ) );
#21842 = APPLICATION_CONTEXT ( 'automotive_design' ) ;
#21843 = EDGE_CURVE ( 'NONE', #369, #20892, #11080, .T. ) ;
#21844 = DIRECTION ( 'NONE',  ( 0.01292394549866738782, 0.005513023399720468239, 0.9999012842304692006 ) ) ;
#21845 = CYLINDRICAL_SURFACE ( 'NONE', #1519, 101.0000000000000000 ) ;
#21846 = ORIENTED_EDGE ( 'NONE', *, *, #17285, .T. ) ;
#21847 = CARTESIAN_POINT ( 'NONE',  ( -16.49317536315907162, 164.3238961432036263, 299.8727917740469593 ) ) ;
#21848 = EDGE_LOOP ( 'NONE', ( #9039, #11085, #6165 ) ) ;
#21849 = VERTEX_POINT ( 'NONE', #11843 ) ;
#21850 = CARTESIAN_POINT ( 'NONE',  ( 47.86793869886106734, 110.7138355817038615, -44.79621871236214048 ) ) ;
#21851 = CARTESIAN_POINT ( 'NONE',  ( 63.76679636398969819, 169.4762627770265340, -95.83069122569631304 ) ) ;
#21852 = EDGE_LOOP ( 'NONE', ( #1122, #2800, #12612, #14877 ) ) ;
#21853 = LINE ( 'NONE', #4293, #12508 ) ;
#21854 =( NAMED_UNIT ( * ) SI_UNIT ( $, .STERADIAN. ) SOLID_ANGLE_UNIT ( ) );
#21855 = CARTESIAN_POINT ( 'NONE',  ( 29.05310264022292799, 95.51270090492249665, 81.29561921768979005 ) ) ;
#21856 = DIRECTION ( 'NONE',  ( 0.9934404589540162256, 0.1135548637187055315, -0.01346653032743023309 ) ) ;
#21857 = DIRECTION ( 'NONE',  ( -0.9909299940865187173, 0.1338359446631173233, 0.01207007604876291287 ) ) ;
#21858 = EDGE_CURVE ( 'NONE', #15773, #21621, #17223, .T. ) ;
#21859 = ORIENTED_EDGE ( 'NONE', *, *, #22366, .T. ) ;
#21860 = CARTESIAN_POINT ( 'NONE',  ( 2.889559250536359425, 175.2456879812082775, 299.5620475989642841 ) ) ;
#21861 = DIRECTION ( 'NONE',  ( 0.4341175610356616810, -0.0005156135821068885683, 0.9008560802609273388 ) ) ;
#21862 = DIRECTION ( 'NONE',  ( 0.01292394549866738782, 0.005513023399720468239, 0.9999012842304692006 ) ) ;
#21863 = LINE ( 'NONE', #13303, #5650 ) ;
#21864 = CARTESIAN_POINT ( 'NONE',  ( 91.76144944056427732, 79.85812038789160283, -31.26012496009718333 ) ) ;
#21865 = FACE_OUTER_BOUND ( 'NONE', #18601, .T. ) ;
#21866 = ORIENTED_EDGE ( 'NONE', *, *, #10667, .F. ) ;
#21867 = CARTESIAN_POINT ( 'NONE',  ( 48.81886788476170125, 189.4982446786774517, -91.70508077603835773 ) ) ;
#21868 = ADVANCED_FACE ( 'NONE', ( #18833 ), #20228, .T. ) ;
#21869 = EDGE_LOOP ( 'NONE', ( #19285, #21524, #13909, #20442 ) ) ;
#21870 = FACE_OUTER_BOUND ( 'NONE', #8464, .T. ) ;
#21871 = CARTESIAN_POINT ( 'NONE',  ( -9.537647826102183757, 184.6943640793454904, 308.0092459792239765 ) ) ;
#21872 = AXIS2_PLACEMENT_3D ( 'NONE', #13684, #17229, #6333 ) ;
#21873 = ORIENTED_EDGE ( 'NONE', *, *, #2338, .F. ) ;
#21874 = EDGE_LOOP ( 'NONE', ( #2887, #3567, #7912, #10884 ) ) ;
#21875 = LINE ( 'NONE', #13319, #3378 ) ;
#21876 = DIRECTION ( 'NONE',  ( -0.01292394549866695240, -0.005513023399725255208, -0.9999012842304693116 ) ) ;
#21877 = AXIS2_PLACEMENT_3D ( 'NONE', #16587, #7710, #21584 ) ;
#21878 = DIRECTION ( 'NONE',  ( 0.9999164797902015955, 6.965998958219364448E-18, -0.01292414190464157182 ) ) ;
#21879 = ADVANCED_FACE ( 'NONE', ( #10111 ), #8365, .T. ) ;
#21880 = EDGE_CURVE ( 'NONE', #7401, #7916, #15411, .T. ) ;
#21881 = LINE ( 'NONE', #11351, #17001 ) ;
#21882 = B_SPLINE_CURVE_WITH_KNOTS ( 'NONE', 3,
 ( #7905, #4222, #18254, #14942, #6068, #21885, #799, #13434, #6182, #11474, #21663, #5951, #20402, #4328, #13207, #9854, #15045, #4561, #12990, #18585, #11249, #11354, #6303, #18361, #19956, #18686, #16434, #22001, #16546, #13328, #7796, #2511, #9515, #4660, #14829, #21781, #2631, #13101, #9643, #20177, #4450, #18481 ),
 .UNSPECIFIED., .F., .F.,
 ( 4, 2, 2, 2, 2, 2, 2, 2, 2, 2, 2, 2, 2, 2, 2, 2, 2, 2, 2, 2, 4 ),
 ( 0.005089968351066945750, 0.006687358310421633728, 0.008284748269776320839, 0.009882138229131007950, 0.01068083320880843651, 0.01147952818848586506, 0.01307691814784075687, 0.01387561312751814033, 0.01467430810719552031, 0.01627169806655027681, 0.01707039304622773312, 0.01786908802590518597, 0.01946647798526022002, 0.02106386794461525408, 0.02266125790397028814, 0.02425864786332531872, 0.02585603782268035278, 0.02745342778203538683, 0.02905081774139042089, 0.02984951272106796047, 0.03064820770074549311 ),
 .UNSPECIFIED. ) ;
#21883 = VERTEX_POINT ( 'NONE', #15633 ) ;
#21884 = DIRECTION ( 'NONE',  ( -0.01292394549866740343, -0.005513023399721215904, -0.9999012842304693116 ) ) ;
#21885 = CARTESIAN_POINT ( 'NONE',  ( -13.98211408154155855, 180.1057412711771804, 320.5253968426166580 ) ) ;
#21886 = EDGE_LOOP ( 'NONE', ( #5952, #11499, #4078, #3905, #21080 ) ) ;
#21887 = ORIENTED_EDGE ( 'NONE', *, *, #20990, .T. ) ;
#21888 = CARTESIAN_POINT ( 'NONE',  ( -106.7230861007157756, 79.13476608364851472, -26.64972274501326055 ) ) ;
#21889 = SHAPE_REPRESENTATION ( 'Angle Locking Side Clamp', ( #6292 ), #13288 ) ;
#21890 = CARTESIAN_POINT ( 'NONE',  ( 64.07473967894682687, 105.0000000000000000, -72.00569783435743432 ) ) ;
#21891 = CARTESIAN_POINT ( 'NONE',  ( -2.888085112683865585, 86.22276635713151904, 75.12774216256403292 ) ) ;
#21892 = ORIENTED_EDGE ( 'NONE', *, *, #18668, .T. ) ;
#21893 = VERTEX_POINT ( 'NONE', #11612 ) ;
#21894 = FACE_OUTER_BOUND ( 'NONE', #21805, .T. ) ;
#21895 = CIRCLE ( 'NONE', #9833, 3.047499999999998987 ) ;
#21896 = CARTESIAN_POINT ( 'NONE',  ( -9.583079365734665345, 187.2593659366937686, 308.0359405774264587 ) ) ;
#21897 = DIRECTION ( 'NONE',  ( -0.9999164797902015955, 0.000000000000000000, 0.01292414190464162733 ) ) ;
#21898 = AXIS2_PLACEMENT_3D ( 'NONE', #22470, #1715, #6870 ) ;
#21899 = ORIENTED_EDGE ( 'NONE', *, *, #12866, .T. ) ;
#21900 = B_SPLINE_CURVE_WITH_KNOTS ( 'NONE', 3,
 ( #15438, #18635, #3222, #13818 ),
 .UNSPECIFIED., .F., .F.,
 ( 4, 4 ),
 ( 2.380735202022725770E-07, 0.002921157996827033858 ),
 .UNSPECIFIED. ) ;
#21901 = LINE ( 'NONE', #13108, #3632 ) ;
#21902 = CARTESIAN_POINT ( 'NONE',  ( -89.81568892019076600, 87.99790937754146114, 50.78728647262676787 ) ) ;
#21903 = APPLICATION_PROTOCOL_DEFINITION ( 'draft international standard', 'automotive_design', 1998, #10138 ) ;
#21904 = CIRCLE ( 'NONE', #2127, 6.499999999999998224 ) ;
#21905 = ORIENTED_EDGE ( 'NONE', *, *, #4286, .F. ) ;
#21906 = CYLINDRICAL_SURFACE ( 'NONE', #19755, 2.000000000000001776 ) ;
#21907 = ADVANCED_FACE ( 'NONE', ( #17022 ), #9977, .T. ) ;
#21908 = CARTESIAN_POINT ( 'NONE',  ( -51.39706450756224854, 113.2585145316183883, -43.52722682608234805 ) ) ;
#21909 = ORIENTED_EDGE ( 'NONE', *, *, #12907, .F. ) ;
#21910 = DIRECTION ( 'NONE',  ( 0.9934404589540163366, 0.1135548637187057258, -0.01346653032743036146 ) ) ;
#21911 = DIRECTION ( 'NONE',  ( -0.01292394549866737220, -0.005513023399721000799, -0.9999012842304692006 ) ) ;
#21912 = EDGE_LOOP ( 'NONE', ( #5061, #15224, #2077, #572 ) ) ;
#21913 = LINE ( 'NONE', #4803, #22545 ) ;
#21914 = AXIS2_PLACEMENT_3D ( 'NONE', #1335, #22422, #4638 ) ;
#21915 = FACE_OUTER_BOUND ( 'NONE', #6491, .T. ) ;
#21916 = ORIENTED_EDGE ( 'NONE', *, *, #5894, .T. ) ;
#21917 = LINE ( 'NONE', #6209, #12485 ) ;
#21918 = EDGE_LOOP ( 'NONE', ( #16700, #3862, #2781, #18297 ) ) ;
#21919 = CARTESIAN_POINT ( 'NONE',  ( 48.79389705813401434, 169.4872888238259634, -93.63702652866572862 ) ) ;
#21920 = CARTESIAN_POINT ( 'NONE',  ( 85.84563054365274581, 105.0000000000000142, 68.77965573371083963 ) ) ;
#21921 = DIRECTION ( 'NONE',  ( -0.9909299940865182732, 0.1338359446631206262, 0.01207007604876868950 ) ) ;
#21922 = DIRECTION ( 'NONE',  ( 7.125109674161246868E-05, -0.9999848031710252272, 0.005512562950850154186 ) ) ;
#21923 = ORIENTED_EDGE ( 'NONE', *, *, #13658, .T. ) ;
#21924 = DIRECTION ( 'NONE',  ( 0.01292394549866739996, 0.005513023399721131770, 0.9999012842304692006 ) ) ;
#21925 = FILL_AREA_STYLE ('',( #10014 ) ) ;
#21926 = ORIENTED_EDGE ( 'NONE', *, *, #18923, .T. ) ;
#21927 = DIRECTION ( 'NONE',  ( -0.01035335185279127358, -0.005513005182357338940, -0.9999312050732649393 ) ) ;
#21928 = AXIS2_PLACEMENT_3D ( 'NONE', #18179, #6093, #13119 ) ;
#21929 = ORIENTED_EDGE ( 'NONE', *, *, #15326, .T. ) ;
#21930 = ORIENTED_EDGE ( 'NONE', *, *, #21023, .T. ) ;
#21931 = CARTESIAN_POINT ( 'NONE',  ( -90.16809648441123670, 87.14955667014993423, 51.30734591929146404 ) ) ;
#21932 = B_SPLINE_CURVE_WITH_KNOTS ( 'NONE', 3,
 ( #2472, #18317, #9822, #16629, #13403, #2708, #985, #6258, #4291, #879, #4185, #19915, #20374, #5911 ),
 .UNSPECIFIED., .F., .F.,
 ( 4, 2, 2, 2, 2, 2, 4 ),
 ( 0.0002285844881980661123, 0.001015112171707181982, 0.001801639855216298014, 0.002194903696970858849, 0.002588167538725419468, 0.002981431380479980520, 0.003374695222234541138 ),
 .UNSPECIFIED. ) ;
#21933 = LINE ( 'NONE', #8589, #1997 ) ;
#21934 = ORIENTED_EDGE ( 'NONE', *, *, #13338, .T. ) ;
#21935 = EDGE_CURVE ( 'NONE', #2060, #3864, #10338, .T. ) ;
#21936 = CARTESIAN_POINT ( 'NONE',  ( 1.717753310876226625, 55.00000000000000000, 109.6869605904137330 ) ) ;
#21937 = CARTESIAN_POINT ( 'NONE',  ( -6.504117289611111019, 188.9465505160917473, 275.5474451934275635 ) ) ;
#21938 = AXIS2_PLACEMENT_3D ( 'NONE', #17877, #2110, #9221 ) ;
#21939 = EDGE_CURVE ( 'NONE', #1692, #680, #22050, .T. ) ;
#21940 = CARTESIAN_POINT ( 'NONE',  ( -88.18626700604421842, 88.78700735547668899, 50.43357012433555298 ) ) ;
#21941 = CARTESIAN_POINT ( 'NONE',  ( 79.92740525950247843, 55.00000000000000000, -6.133505399301337313 ) ) ;
#21942 = DIRECTION ( 'NONE',  ( -0.009138748381789078140, 0.7071067811865487940, -0.7070477234798315802 ) ) ;
#21943 = ORIENTED_EDGE ( 'NONE', *, *, #4897, .F. ) ;
#21944 = CIRCLE ( 'NONE', #19024, 6.500000000000013323 ) ;
#21945 = CARTESIAN_POINT ( 'NONE',  ( 9.391523084377633168, 190.1646184555798129, 274.7467018831596306 ) ) ;
#21946 = CARTESIAN_POINT ( 'NONE',  ( 20.36766808887146851, 182.1959104846870616, 311.9746127290063100 ) ) ;
#21947 = DIRECTION ( 'NONE',  ( 0.2320196626118057881, -0.9719970830534312434, 0.03726320835790866703 ) ) ;
#21948 = CARTESIAN_POINT ( 'NONE',  ( -70.91392079944854743, 72.00000000000000000, -84.09052168258642723 ) ) ;
#21949 = EDGE_LOOP ( 'NONE', ( #2542, #12936, #18901, #12760, #5862 ) ) ;
#21950 = EDGE_CURVE ( 'NONE', #13554, #22043, #10718, .T. ) ;
#21951 = FACE_OUTER_BOUND ( 'NONE', #14181, .T. ) ;
#21952 = CARTESIAN_POINT ( 'NONE',  ( -10.00417312871659270, 187.8841867195822601, 308.1584149291320500 ) ) ;
#21953 = CLOSED_SHELL ( 'NONE', ( #1565, #22599, #5285, #4339, #19991, #1791, #4300, #13469, #7576, #3457, #6538, #16018, #20768, #10973, #17079, #19038, #21970, #10612, #13862, #7924, #14101, #4490, #8122, #7122, #10465 ) ) ;
#21954 = ORIENTED_EDGE ( 'NONE', *, *, #18333, .T. ) ;
#21955 = DIRECTION ( 'NONE',  ( 0.9999164797902017066, 0.000000000000000000, -0.01292414190463751951 ) ) ;
#21956 = VECTOR ( 'NONE', #8784, 1000.000000000000114 ) ;
#21957 = ORIENTED_EDGE ( 'NONE', *, *, #12149, .T. ) ;
#21958 = CARTESIAN_POINT ( 'NONE',  ( 48.60410837317779453, 111.9941758084687109, -44.81279311089502926 ) ) ;
#21959 = DIRECTION ( 'NONE',  ( -2.025474946048326158E-22, 1.000000000000000000, -1.876735158486679638E-22 ) ) ;
#21960 = ADVANCED_FACE ( 'NONE', ( #4799 ), #13348, .F. ) ;
#21961 = ORIENTED_EDGE ( 'NONE', *, *, #4872, .F. ) ;
#21962 = AXIS2_PLACEMENT_3D ( 'NONE', #9405, #16445, #4233 ) ;
#21963 = ORIENTED_EDGE ( 'NONE', *, *, #4298, .F. ) ;
#21964 = CARTESIAN_POINT ( 'NONE',  ( 78.28083514950689903, 75.12313863457447383, -5.849292866322538309 ) ) ;
#21965 = CARTESIAN_POINT ( 'NONE',  ( -89.67405064417086180, 69.73069950987664356, 63.42040036413745696 ) ) ;
#21966 = EDGE_CURVE ( 'NONE', #13016, #883, #13557, .T. ) ;
#21967 = CARTESIAN_POINT ( 'NONE',  ( -110.0212991616528768, 74.99906874937914836, -0.8747890471060359996 ) ) ;
#21968 = FACE_OUTER_BOUND ( 'NONE', #298, .T. ) ;
#21969 = CARTESIAN_POINT ( 'NONE',  ( 26.59130080239608773, 189.4003865961453812, -109.1693451709174099 ) ) ;
#21970 = ADVANCED_FACE ( 'NONE', ( #13680 ), #16896, .T. ) ;
#21971 = ORIENTED_EDGE ( 'NONE', *, *, #9747, .F. ) ;
#21972 = EDGE_CURVE ( 'NONE', #20464, #665, #22010, .T. ) ;
#21973 = EDGE_LOOP ( 'NONE', ( #4661, #13875, #20753, #12991, #17736, #19413 ) ) ;
#21974 = CARTESIAN_POINT ( 'NONE',  ( -68.71681667565952978, 72.00000000000000000, 85.89527988174785378 ) ) ;
#21975 = DIRECTION ( 'NONE',  ( 0.9999164797902015955, 6.965998958219364448E-18, -0.01292414190464157182 ) ) ;
#21976 = CARTESIAN_POINT ( 'NONE',  ( -51.82743751170760049, 114.6914167488026095, 172.2189919798578899 ) ) ;
#21977 = VECTOR ( 'NONE', #4106, 1000.000000000000114 ) ;
#21978 = EDGE_CURVE ( 'NONE', #20892, #12459, #6765, .T. ) ;
#21979 = CARTESIAN_POINT ( 'NONE',  ( 90.67285013207080624, 77.76891457534604513, -32.19520807900808279 ) ) ;
#21980 = CIRCLE ( 'NONE', #12114, 2.000000000000004885 ) ;
#21981 = CARTESIAN_POINT ( 'NONE',  ( -88.23797876370683468, 94.47357722488187903, 47.15541951427123024 ) ) ;
#21982 = ORIENTED_EDGE ( 'NONE', *, *, #11201, .F. ) ;
#21983 = CARTESIAN_POINT ( 'NONE',  ( 48.82059446874842479, 189.4989811950858609, -91.57149822991706856 ) ) ;
#21984 = VERTEX_POINT ( 'NONE', #20770 ) ;
#21985 = DIRECTION ( 'NONE',  ( -0.7084451806051488276, -0.7056452299526765337, 0.01304743355500853977 ) ) ;
#21986 = CIRCLE ( 'NONE', #7718, 20.50000000000000000 ) ;
#21987 = CARTESIAN_POINT ( 'NONE',  ( -14.62647227136777595, 179.3338414634184801, 312.0078474254344769 ) ) ;
#21988 = ORIENTED_EDGE ( 'NONE', *, *, #13013, .F. ) ;
#21989 = EDGE_LOOP ( 'NONE', ( #13278, #1982, #19393, #15304 ) ) ;
#21990 = EDGE_CURVE ( 'NONE', #22275, #5033, #5026, .T. ) ;
#21991 = VECTOR ( 'NONE', #13272, 1000.000000000000114 ) ;
#21992 = PRODUCT_DEFINITION_SHAPE ( 'NONE', 'NONE',  #7900 ) ;
#21993 = CIRCLE ( 'NONE', #17255, 109.9999999999999858 ) ;
#21994 = CARTESIAN_POINT ( 'NONE',  ( -64.99457118636311748, 170.0000000000008242, 0.8400692238025471159 ) ) ;
#21995 = AXIS2_PLACEMENT_3D ( 'NONE', #16408, #2381, #9733 ) ;
#21996 = CARTESIAN_POINT ( 'NONE',  ( -162.0000000000000000, 0.000000000000000000, -9.999999999999978684 ) ) ;
#21997 = ADVANCED_FACE ( 'NONE', ( #6443 ), #13455, .F. ) ;
#21998 = CARTESIAN_POINT ( 'NONE',  ( -64.32311159746099349, 87.99029836822310813, 52.78963101368245248 ) ) ;
#21999 = ORIENTED_EDGE ( 'NONE', *, *, #18153, .F. ) ;
#22000 = CARTESIAN_POINT ( 'NONE',  ( 11.62929739413847408, 187.8579631343771439, 307.7555743005772797 ) ) ;
#22001 = CARTESIAN_POINT ( 'NONE',  ( -14.22642941140435191, 179.9086452483393828, 309.1547204902269641 ) ) ;
#22002 = VERTEX_POINT ( 'NONE', #12638 ) ;
#22003 = DIRECTION ( 'NONE',  ( 0.9999164797902015955, 2.001050586450179636E-22, -0.01292414190464084844 ) ) ;
#22004 = DIRECTION ( 'NONE',  ( 0.9999164797902015955, 2.001050586450177755E-22, -0.01292414190464177999 ) ) ;
#22005 = LINE ( 'NONE', #4565, #8134 ) ;
#22006 = VECTOR ( 'NONE', #17505, 999.9999999999998863 ) ;
#22007 = VERTEX_POINT ( 'NONE', #10669 ) ;
#22008 = AXIS2_PLACEMENT_3D ( 'NONE', #6840, #19126, #19011 ) ;
#22009 = FACE_OUTER_BOUND ( 'NONE', #5294, .T. ) ;
#22010 = CIRCLE ( 'NONE', #12139, 75.00000000000002842 ) ;
#22011 = CARTESIAN_POINT ( 'NONE',  ( -9.995692194476635706, 187.8898849410517471, 308.1575541326492953 ) ) ;
#22012 = EDGE_CURVE ( 'NONE', #18467, #11266, #19614, .T. ) ;
#22013 = VECTOR ( 'NONE', #19908, 999.9999999999998863 ) ;
#22014 = ADVANCED_FACE ( 'NONE', ( #3436 ), #10557, .F. ) ;
#22015 = ORIENTED_EDGE ( 'NONE', *, *, #8750, .F. ) ;
#22016 = LINE ( 'NONE', #22136, #13912 ) ;
#22017 = CARTESIAN_POINT ( 'NONE',  ( -10.80139054985347968, 105.7231500355213853, 131.4989882570862676 ) ) ;
#22018 = APPLICATION_PROTOCOL_DEFINITION ( 'draft international standard', 'automotive_design', 1998, #12043 ) ;
#22020 = ORIENTED_EDGE ( 'NONE', *, *, #798, .F. ) ;
#22019 = ORIENTED_EDGE ( 'NONE', *, *, #14300, .T. ) ;
#22021 = CARTESIAN_POINT ( 'NONE',  ( 0.000000000000000000, 29.00000000000000711, 0.000000000000000000 ) ) ;
#22022 = AXIS2_PLACEMENT_3D ( 'NONE', #19240, #19463, #15941 ) ;
#22023 = CARTESIAN_POINT ( 'NONE',  ( 90.40889375659912730, 78.43035437438885538, -33.17122784026042837 ) ) ;
#22024 = VERTEX_POINT ( 'NONE', #5255 ) ;
#22025 = CYLINDRICAL_SURFACE ( 'NONE', #3737, 2.000000000000001332 ) ;
#22026 = FACE_OUTER_BOUND ( 'NONE', #4838, .T. ) ;
#22027 = CIRCLE ( 'NONE', #22386, 7.500000000000002665 ) ;
#22028 = CYLINDRICAL_SURFACE ( 'NONE', #7557, 7.499999999999991118 ) ;
#22029 = DIRECTION ( 'NONE',  ( -0.01292414190464117631, -5.551059884324762197E-17, -0.9999164797902017066 ) ) ;
#22030 = CIRCLE ( 'NONE', #4122, 9.000000000000001776 ) ;
#22031 = CARTESIAN_POINT ( 'NONE',  ( -105.4334892372614121, 77.12912189496637438, 31.36525700924958926 ) ) ;
#22032 = VERTEX_POINT ( 'NONE', #9036 ) ;
#22033 = CARTESIAN_POINT ( 'NONE',  ( 6.781388072971600067, 37.00000000000000711, -83.91926714759891581 ) ) ;
#22034 = VECTOR ( 'NONE', #6969, 1000.000000000000114 ) ;
#22035 = VERTEX_POINT ( 'NONE', #3884 ) ;
#22036 = CYLINDRICAL_SURFACE ( 'NONE', #22385, 6.000000000000000888 ) ;
#22037 = CARTESIAN_POINT ( 'NONE',  ( -157.5176307659779411, 1.999999999999998224, 60.94675664190624076 ) ) ;
#22038 = DIRECTION ( 'NONE',  ( -2.025474946048326158E-22, 1.000000000000000000, -1.876735158486678933E-22 ) ) ;
#22039 = CARTESIAN_POINT ( 'NONE',  ( -54.52327687265817246, 20.00000000000000000, -111.3697098814011781 ) ) ;
#22040 = ORIENTED_EDGE ( 'NONE', *, *, #6962, .T. ) ;
#22041 = DIRECTION ( 'NONE',  ( -0.9999164797902015955, -6.965998958219364448E-18, 0.01292414190464157182 ) ) ;
#22042 =( LENGTH_UNIT ( ) NAMED_UNIT ( * ) SI_UNIT ( .MILLI., .METRE. ) );
#22043 = VERTEX_POINT ( 'NONE', #7218 ) ;
#22044 = TOROIDAL_SURFACE ( 'NONE', #1184, 124.0000000000000000, 2.000000000000000000 ) ;
#22045 = ADVANCED_FACE ( 'NONE', ( #19389 ), #1945, .T. ) ;
#22046 = DIRECTION ( 'NONE',  ( -0.01292394549866741904, -0.005513023399721091004, -0.9999012842304693116 ) ) ;
#22047 = EDGE_CURVE ( 'NONE', #20235, #8789, #12178, .T. ) ;
#22048 = CARTESIAN_POINT ( 'NONE',  ( 45.75746115295205385, 168.8246939296725202, 58.31253523502198988 ) ) ;
#22049 = ORIENTED_EDGE ( 'NONE', *, *, #14121, .F. ) ;
#22050 = CIRCLE ( 'NONE', #5938, 6.000000000000004441 ) ;
#22051 = FACE_OUTER_BOUND ( 'NONE', #2663, .T. ) ;
#22052 = CARTESIAN_POINT ( 'NONE',  ( -88.16496929303228569, 88.40829394340927649, 52.78344489490578439 ) ) ;
#22053 = AXIS2_PLACEMENT_3D ( 'NONE', #19639, #17849, #21245 ) ;
#22054 = DIRECTION ( 'NONE',  ( 0.1351880940536942799, -0.9908129862407182298, 0.003715578404455081168 ) ) ;
#22055 = ORIENTED_EDGE ( 'NONE', *, *, #15287, .T. ) ;
#22056 = DIRECTION ( 'NONE',  ( 0.9999164797902015955, 6.965998958219364448E-18, -0.01292414190464157182 ) ) ;
#22057 = DIRECTION ( 'NONE',  ( 0.009188991635466195809, -0.7031977391749432149, 0.7109349492407668336 ) ) ;
#22058 = CONICAL_SURFACE ( 'NONE', #4099, 3.399999999999986144, 1.029744258676653201 ) ;
#22059 = CARTESIAN_POINT ( 'NONE',  ( -88.18538491329667295, 88.84369698205085797, 50.55255461122708027 ) ) ;
#22060 = CARTESIAN_POINT ( 'NONE',  ( -91.93574473583122142, 79.05185923607193388, 28.63941780214905108 ) ) ;
#22061 = CIRCLE ( 'NONE', #2280, 110.0000000000000000 ) ;
#22062 = CIRCLE ( 'NONE', #14413, 7.499999999999992006 ) ;
#22063 = DIRECTION ( 'NONE',  ( 7.125109674364534776E-05, -0.9999848031710252272, 0.005512562950849704893 ) ) ;
#22064 = ORIENTED_EDGE ( 'NONE', *, *, #14294, .T. ) ;
#22065 = DIRECTION ( 'NONE',  ( -0.9999164797902015955, -6.965998958219364448E-18, 0.01292414190464157182 ) ) ;
#22066 = CARTESIAN_POINT ( 'NONE',  ( 17.02725847016130345, 185.2342960137961825, 319.7397003021923183 ) ) ;
#22067 = CARTESIAN_POINT ( 'NONE',  ( 1.364374947835851710E-14, 55.00000000000000000, -9.836440897896405351E-15 ) ) ;
#22068 = CARTESIAN_POINT ( 'NONE',  ( -1.632550740186646365, 142.7036636415817838, 274.8672572718561469 ) ) ;
#22069 = EDGE_LOOP ( 'NONE', ( #1696, #2862, #483, #10056 ) ) ;
#22070 = DIRECTION ( 'NONE',  ( 1.000000000000000000, 0.000000000000000000, 0.000000000000000000 ) ) ;
#22071 = AXIS2_PLACEMENT_3D ( 'NONE', #10221, #17224, #1719 ) ;
#22072 = DIRECTION ( 'NONE',  ( -0.01292394549866731843, -0.005513023399720594006, -0.9999012842304693116 ) ) ;
#22073 = DIRECTION ( 'NONE',  ( 0.9934404589540162256, 0.1135548637187056842, -0.01346653032743081423 ) ) ;
#22074 = EDGE_LOOP ( 'NONE', ( #16761, #16033, #3183, #13715 ) ) ;
#22075 = CARTESIAN_POINT ( 'NONE',  ( -11.58738668730085841, 185.5101712897686355, 277.0082871630683030 ) ) ;
#22076 = ORIENTED_EDGE ( 'NONE', *, *, #21689, .F. ) ;
#22077 = ADVANCED_FACE ( 'NONE', ( #10896 ), #17699, .F. ) ;
#22078 = EDGE_LOOP ( 'NONE', ( #18671, #17388 ) ) ;
#22079 = VECTOR ( 'NONE', #1348, 1000.000000000000000 ) ;
#22080 = DIRECTION ( 'NONE',  ( -0.9232306267972774094, 0.000000000000000000, 0.3842462878721227826 ) ) ;
#22081 = AXIS2_PLACEMENT_3D ( 'NONE', #11006, #18035, #2283 ) ;
#22082 = CARTESIAN_POINT ( 'NONE',  ( -2.067862704742604141, 72.00000000000000000, -159.9866367664322979 ) ) ;
#22083 = FILL_AREA_STYLE_COLOUR ( '', #10578 ) ;
#22084 = DIRECTION ( 'NONE',  ( -7.176269450075758328E-19, 1.000000000000000000, -5.550596000020002074E-17 ) ) ;
#22085 = CARTESIAN_POINT ( 'NONE',  ( 105.8287943736950609, 79.03195428549129531, -30.00479353936319882 ) ) ;
#22086 = CARTESIAN_POINT ( 'NONE',  ( -1.163172771417702700, 37.00000000000000711, -89.99248318111824574 ) ) ;
#22087 = ADVANCED_FACE ( 'NONE', ( #3774 ), #13893, .T. ) ;
#22088 = CARTESIAN_POINT ( 'NONE',  ( -41.15169610061244754, 101.1708071963161615, 65.90309081746964637 ) ) ;
#22089 = CARTESIAN_POINT ( 'NONE',  ( 12.82909088464482217, 190.5347596758964244, 307.8494772114028137 ) ) ;
#22090 = CYLINDRICAL_SURFACE ( 'NONE', #4379, 2.000000000000000000 ) ;
#22091 = CARTESIAN_POINT ( 'NONE',  ( 41.48434878520766489, 95.06228642946297214, 83.37923770918371247 ) ) ;
#22092 = DIRECTION ( 'NONE',  ( 7.125109674159588039E-05, -0.9999848031710253382, 0.005512562950848870491 ) ) ;
#22093 = CIRCLE ( 'NONE', #16643, 2.272904689641356057 ) ;
#22094 = CARTESIAN_POINT ( 'NONE',  ( -56.14790736339946164, 143.5743091050289024, 104.9804413797129286 ) ) ;
#22095 = CIRCLE ( 'NONE', #12232, 9.000000000000000000 ) ;
#22096 = EDGE_CURVE ( 'NONE', #5718, #18167, #17649, .T. ) ;
#22097 = CARTESIAN_POINT ( 'NONE',  ( 92.19651396575548574, 79.04398536194628377, -28.61663131200300469 ) ) ;
#22098 = FACE_OUTER_BOUND ( 'NONE', #19913, .T. ) ;
#22099 = ORIENTED_EDGE ( 'NONE', *, *, #3112, .T. ) ;
#22100 = ORIENTED_EDGE ( 'NONE', *, *, #6348, .T. ) ;
#22101 = DIRECTION ( 'NONE',  ( 7.125109673814330634E-05, -0.9999848031710252272, 0.005512562950850199289 ) ) ;
#22102 = CARTESIAN_POINT ( 'NONE',  ( -10.39997831424552110, 184.0167981025738868, 305.6179304391126834 ) ) ;
#22103 = ORIENTED_EDGE ( 'NONE', *, *, #5841, .T. ) ;
#22104 = CIRCLE ( 'NONE', #7839, 11.00000000000000178 ) ;
#22105 = EDGE_CURVE ( 'NONE', #18877, #1288, #16925, .T. ) ;
#22106 = ORIENTED_EDGE ( 'NONE', *, *, #14591, .F. ) ;
#22107 = EDGE_CURVE ( 'NONE', #16756, #10313, #10793, .T. ) ;
#22108 = CIRCLE ( 'NONE', #4515, 4.999999999999997335 ) ;
#22109 = CYLINDRICAL_SURFACE ( 'NONE', #4463, 95.00000000000004263 ) ;
#22110 = EDGE_LOOP ( 'NONE', ( #10720, #2162, #20765, #17850 ) ) ;
#22111 = DIRECTION ( 'NONE',  ( 0.9232306267972768543, 0.000000000000000000, -0.3842462878721243924 ) ) ;
#22112 = EDGE_CURVE ( 'NONE', #20716, #13764, #21000, .T. ) ;
#22113 = DIRECTION ( 'NONE',  ( -0.000000000000000000, -1.000000000000000000, 0.000000000000000000 ) ) ;
#22114 = CARTESIAN_POINT ( 'NONE',  ( -40.54264932485133954, 123.7663955596447352, -41.72526100787018777 ) ) ;
#22115 = EDGE_LOOP ( 'NONE', ( #14249, #1062, #4223, #22399 ) ) ;
#22116 = VECTOR ( 'NONE', #4723, 1000.000000000000114 ) ;
#22117 = EDGE_CURVE ( 'NONE', #21200, #12626, #11039, .T. ) ;
#22118 = ORIENTED_EDGE ( 'NONE', *, *, #14196, .F. ) ;
#22119 = ADVANCED_FACE ( 'NONE', ( #7106 ), #222, .T. ) ;
#22120 = DIRECTION ( 'NONE',  ( -0.4397038457472313144, 0.000000000000000000, 0.8981428216242086648 ) ) ;
#22121 = CARTESIAN_POINT ( 'NONE',  ( -106.8361484267444723, 79.08880628745897923, -26.19276530885237975 ) ) ;
#22122 = CARTESIAN_POINT ( 'NONE',  ( -41.47069032946998846, 166.0668615304125808, 273.1833561390217824 ) ) ;
#22123 = DIRECTION ( 'NONE',  ( -0.01292394549866741384, -0.005513023399721118760, -0.9999012842304692006 ) ) ;
#22124 = AXIS2_PLACEMENT_3D ( 'NONE', #12801, #20011, #9451 ) ;
#22125 = ORIENTED_EDGE ( 'NONE', *, *, #8787, .T. ) ;
#22126 = FACE_OUTER_BOUND ( 'NONE', #12844, .T. ) ;
#22127 = AXIS2_PLACEMENT_3D ( 'NONE', #3462, #13811, #5165 ) ;
#22128 = CARTESIAN_POINT ( 'NONE',  ( -38.56531521350735403, 165.8559883853732515, 234.8931899347302874 ) ) ;
#22129 = CARTESIAN_POINT ( 'NONE',  ( 13.62697418300035679, 144.0917254245173353, 275.5345564924090809 ) ) ;
#22130 = EDGE_CURVE ( 'NONE', #19552, #591, #5366, .T. ) ;
#22131 = CARTESIAN_POINT ( 'NONE',  ( 79.99331838321614896, 54.99999999999999289, -1.033931352371314949 ) ) ;
#22132 = EDGE_CURVE ( 'NONE', #14396, #1325, #9658, .T. ) ;
#22133 = SPHERICAL_SURFACE ( 'NONE', #11155, 2.000000000000000000 ) ;
#22134 = EDGE_LOOP ( 'NONE', ( #13009, #16767, #2474, #6139 ) ) ;
#22135 = VECTOR ( 'NONE', #2801, 1000.000000000000114 ) ;
#22136 = CARTESIAN_POINT ( 'NONE',  ( -45.12496756436068068, 166.3499139106832558, 244.2261648130215690 ) ) ;
#22137 = DIRECTION ( 'NONE',  ( -0.01292394549866738782, -0.005513023399720700692, -0.9999012842304693116 ) ) ;
#22138 = APPLICATION_PROTOCOL_DEFINITION ( 'draft international standard', 'automotive_design', 1998, #16035 ) ;
#22139 = VECTOR ( 'NONE', #19592, 1000.000000000000000 ) ;
#22141 = EDGE_LOOP ( 'NONE', ( #8018, #14667, #8768 ) ) ;
#22140 = VERTEX_POINT ( 'NONE', #12515 ) ;
#22142 = CIRCLE ( 'NONE', #15968, 14.99999999999997691 ) ;
#22143 = DIRECTION ( 'NONE',  ( 0.9934404589540163366, 0.1135548637187060866, -0.01346653032743036840 ) ) ;
#22144 = CARTESIAN_POINT ( 'NONE',  ( -52.45778058759690765, 111.9218655230933734, -46.78044295554445142 ) ) ;
#22145 = ORIENTED_EDGE ( 'NONE', *, *, #3026, .T. ) ;
#22146 = DIRECTION ( 'NONE',  ( -2.025474946048326158E-22, 1.000000000000000000, -1.876735158486679638E-22 ) ) ;
#22147 = DIRECTION ( 'NONE',  ( 0.01292394549866742424, 0.005513023399720750999, 0.9999012842304693116 ) ) ;
#22148 = LINE ( 'NONE', #9666, #1690 ) ;
#22149 = DIRECTION ( 'NONE',  ( -0.9999164797902015955, -2.001050586498092550E-22, 0.01292414190464117457 ) ) ;
#22151 = DIRECTION ( 'NONE',  ( -0.01292394549866737220, -0.005513023399721000799, -0.9999012842304692006 ) ) ;
#22150 =( REPRESENTATION_RELATIONSHIP ('NONE','NONE', #11808, #17373 ) REPRESENTATION_RELATIONSHIP_WITH_TRANSFORMATION ( #12051 )SHAPE_REPRESENTATION_RELATIONSHIP( ) );
#22152 = VERTEX_POINT ( 'NONE', #6864 ) ;
#22153 = ADVANCED_FACE ( 'NONE', ( #16296 ), #765, .F. ) ;
#22154 = LINE ( 'NONE', #7829, #3272 ) ;
#22155 = DIRECTION ( 'NONE',  ( -0.005493774068846061544, 0.02859024303483492097, -0.9995761183870338629 ) ) ;
#22156 = ORIENTED_EDGE ( 'NONE', *, *, #21561, .F. ) ;
#22157 = LINE ( 'NONE', #14966, #2244 ) ;
#22158 = CARTESIAN_POINT ( 'NONE',  ( 68.31397436809166379, 127.4153035195791119, 255.9758934117053570 ) ) ;
#22159 = AXIS2_PLACEMENT_3D ( 'NONE', #15992, #7227, #8484 ) ;
#22160 = CARTESIAN_POINT ( 'NONE',  ( 106.2089377515399491, 71.86507807689919503, 28.62973177816241588 ) ) ;
#22161 = DIRECTION ( 'NONE',  ( -7.125109674403282806E-05, 0.9999848031710253382, -0.005512562950848280685 ) ) ;
#22162 = ORIENTED_EDGE ( 'NONE', *, *, #9360, .T. ) ;
#22163 = CARTESIAN_POINT ( 'NONE',  ( -66.75560256528235925, 192.1022009597331817, 19.34154534151025118 ) ) ;
#22164 = SURFACE_STYLE_FILL_AREA ( #21925 ) ;
#22165 = VERTEX_POINT ( 'NONE', #9928 ) ;
#22166 = CARTESIAN_POINT ( 'NONE',  ( 5.806620212786450352, 81.64473548815914228, -96.66860143004626593 ) ) ;
#22167 = EDGE_CURVE ( 'NONE', #9211, #18877, #12172, .T. ) ;
#22168 = PLANE ( 'NONE',  #18055 ) ;
#22169 = ORIENTED_EDGE ( 'NONE', *, *, #16442, .F. ) ;
#22170 = CARTESIAN_POINT ( 'NONE',  ( 14.04474127379322468, 113.6585260871128611, 119.4329391803669722 ) ) ;
#22171 = CARTESIAN_POINT ( 'NONE',  ( -88.16451018535700257, 88.36589127631114593, 52.82384857957035251 ) ) ;
#22172 =( BOUNDED_SURFACE ( )  B_SPLINE_SURFACE ( 3, 2, ( 
 ( #20271, #994, #9611 ),
 ( #890, #7881, #14920 ),
 ( #20144, #7980, #15019 ),
 ( #13298, #4534, #18563 ),
 ( #21041, #15254, #15902 ),
 ( #4745, #18662, #3044 ),
 ( #11789, #4642, #6718 ),
 ( #2927, #11669, #6500 ),
 ( #10165, #22207, #5397 ),
 ( #2821, #4865, #21150 ),
 ( #18887, #13512, #10066 ),
 ( #1340, #19315, #1448 ),
 ( #8106, #14057, #13411 ),
 ( #9829, #3575, #145 ) ),
 .UNSPECIFIED., .F., .F., .T. ) 
 B_SPLINE_SURFACE_WITH_KNOTS ( ( 4, 2, 2, 2, 2, 2, 4 ),
 ( 3, 3 ),
 ( -0.01502904264599901930, -0.01127178198449926318, -0.007514521322999507917, -0.005635890992249629854, -0.003757260661499752224, -0.001878630330749874377, 3.469446951953614189E-18 ),
 ( 0.000000000000000000, 1.000000000000000000 ),
 .UNSPECIFIED. ) 
 GEOMETRIC_REPRESENTATION_ITEM ( )  RATIONAL_B_SPLINE_SURFACE ( (
 ( 1.000000000000000000, 1.000000000000000000, 1.000000000000000000),
 ( 1.000000000000000000, 0.9999832193767735911, 1.000000000000000000),
 ( 1.000000000000000000, 0.9943958665397538699, 1.000000000000000000),
 ( 1.000000000000000000, 0.9719875995037652316, 1.000000000000000000),
 ( 1.000000000000000000, 0.9551974090686941032, 1.000000000000000000),
 ( 1.000000000000000000, 0.9207014414826584225, 1.000000000000000000),
 ( 1.000000000000000000, 0.9076211955285893307, 1.000000000000000000),
 ( 1.000000000000000000, 0.8785736512487225536, 1.000000000000000000),
 ( 1.000000000000000000, 0.8625652577268398957, 1.000000000000000000),
 ( 1.000000000000000000, 0.8274118182194920568, 1.000000000000000000),
 ( 1.000000000000000000, 0.8082693262200102424, 1.000000000000000000),
 ( 1.000000000000000000, 0.7665332262304687116, 1.000000000000000000),
 ( 1.000000000000000000, 0.7439399906336684465, 1.000000000000000000),
 ( 1.000000000000000000, 0.7193398003386514139, 1.000000000000000000) ) ) 
 REPRESENTATION_ITEM ( '' )  SURFACE ( )  );
#22173 =( GEOMETRIC_REPRESENTATION_CONTEXT ( 3 ) GLOBAL_UNCERTAINTY_ASSIGNED_CONTEXT ( ( #8989 ) ) GLOBAL_UNIT_ASSIGNED_CONTEXT ( ( #1870, #17749, #5072 ) ) REPRESENTATION_CONTEXT ( 'NONE', 'WORKASPACE' ) );
#22174 = VERTEX_POINT ( 'NONE', #14673 ) ;
#22175 = CARTESIAN_POINT ( 'NONE',  ( -55.33837949231430287, 118.9192529882356268, 167.6120857178884762 ) ) ;
#22176 = FACE_OUTER_BOUND ( 'NONE', #18958, .T. ) ;
#22177 = CARTESIAN_POINT ( 'NONE',  ( -14.37443239621853408, 105.6999454642524654, 127.3358366182947634 ) ) ;
#22178 = ORIENTED_EDGE ( 'NONE', *, *, #14846, .F. ) ;
#22179 = CARTESIAN_POINT ( 'NONE',  ( 1.121675378414710433, 45.00000000000000000, 109.9942809619911799 ) ) ;
#22180 = CARTESIAN_POINT ( 'NONE',  ( -88.18349247326855789, 88.93254284115897690, 50.79801752376152990 ) ) ;
#22181 = CARTESIAN_POINT ( 'NONE',  ( -89.41602473586596034, 79.46258270018842040, 29.93333348547115236 ) ) ;
#22182 = DIRECTION ( 'NONE',  ( -7.176269450075762180E-19, 1.000000000000000000, -5.550596000020001457E-17 ) ) ;
#22183 = EDGE_CURVE ( 'NONE', #2480, #2415, #19275, .T. ) ;
#22184 = ORIENTED_EDGE ( 'NONE', *, *, #10833, .F. ) ;
#22185 = ADVANCED_FACE ( 'NONE', ( #10975 ), #8105, .F. ) ;
#22186 = CARTESIAN_POINT ( 'NONE',  ( -10.92302490886842214, 106.4641486460940456, 120.7954399799814382 ) ) ;
#22187 = CARTESIAN_POINT ( 'NONE',  ( -88.05170339851980543, 72.97786998644572520, 61.56719313945616534 ) ) ;
#22188 = CARTESIAN_POINT ( 'NONE',  ( 64.31784532510161512, 144.7109461922390778, -53.19707257213011076 ) ) ;
#22189 = CARTESIAN_POINT ( 'NONE',  ( -92.05960170301050027, 69.99999999999998579, 60.20821982323565180 ) ) ;
#22190 = CARTESIAN_POINT ( 'NONE',  ( 65.33690683320658366, 190.1463355405889786, 25.64579400984300150 ) ) ;
#22191 = DIRECTION ( 'NONE',  ( 5.440186201345738641E-18, 1.000000000000000000, 1.334940939666364181E-17 ) ) ;
#22192 = CARTESIAN_POINT ( 'NONE',  ( 90.55526626895685638, 99.16641366430587823, 62.44901868852801385 ) ) ;
#22193 = VECTOR ( 'NONE', #1272, 1000.000000000000000 ) ;
#22194 = PRODUCT_DEFINITION_SHAPE ( 'NONE', 'NONE',  #22669 ) ;
#22195 = CARTESIAN_POINT ( 'NONE',  ( 44.31784132852413194, 168.2105890667581605, -53.06813496338226344 ) ) ;
#22196 = CARTESIAN_POINT ( 'NONE',  ( -64.00797876747101611, 100.1288551967107310, 77.17086362122255139 ) ) ;
#22197 = ORIENTED_EDGE ( 'NONE', *, *, #6946, .T. ) ;
#22198 = ORIENTED_EDGE ( 'NONE', *, *, #20974, .T. ) ;
#22199 = ORIENTED_EDGE ( 'NONE', *, *, #15570, .T. ) ;
#22200 = DIRECTION ( 'NONE',  ( -0.8981428216242028917, 0.000000000000000000, -0.4397038457472429718 ) ) ;
#22201 = VERTEX_POINT ( 'NONE', #20266 ) ;
#22202 = CARTESIAN_POINT ( 'NONE',  ( -38.89810712971357987, 72.00000000000000000, 85.50986645835278921 ) ) ;
#22203 = AXIS2_PLACEMENT_3D ( 'NONE', #1827, #6991, #19282 ) ;
#22204 = CARTESIAN_POINT ( 'NONE',  ( -109.5708359150299742, 75.34617192694386745, 10.75083194752825477 ) ) ;
#22205 = EDGE_CURVE ( 'NONE', #10176, #21645, #2922, .T. ) ;
#22206 = CARTESIAN_POINT ( 'NONE',  ( -91.65210746689160715, 71.62127171602891451, -60.82679172889525177 ) ) ;
#22207 = CARTESIAN_POINT ( 'NONE',  ( 17.48198728475768249, 186.4531915267186264, 276.5831127856608305 ) ) ;
#22208 = CARTESIAN_POINT ( 'NONE',  ( 8.108149183870601462, 81.64298031427468061, -87.30072018181317617 ) ) ;
#22209 = CARTESIAN_POINT ( 'NONE',  ( 3.833582208905060185, 166.6352317792379267, 296.5970240496429255 ) ) ;
#22210 = CARTESIAN_POINT ( 'NONE',  ( -5.156377330703347361, 70.80384757729338219, -99.58697729741749072 ) ) ;
#22211 = DIRECTION ( 'NONE',  ( 0.000000000000000000, 0.000000000000000000, -1.000000000000000000 ) ) ;
#22212 = CARTESIAN_POINT ( 'NONE',  ( 92.50365291375123888, 70.32755610701406113, 59.52398455131074684 ) ) ;
#22213 = EDGE_LOOP ( 'NONE', ( #8909, #21819 ) ) ;
#22214 = ORIENTED_EDGE ( 'NONE', *, *, #15406, .F. ) ;
#22215 = CARTESIAN_POINT ( 'NONE',  ( 0.000000000000000000, 25.00000000000000000, 0.000000000000000000 ) ) ;
#22216 = CARTESIAN_POINT ( 'NONE',  ( -8.567848615622622788, 185.3757230055408343, 308.0246556707246555 ) ) ;
#22217 = ORIENTED_EDGE ( 'NONE', *, *, #7074, .T. ) ;
#22218 = CARTESIAN_POINT ( 'NONE',  ( -1.163172771417704698, 69.99999999999998579, -89.99248318111816047 ) ) ;
#22219 = EDGE_LOOP ( 'NONE', ( #7830, #1054, #6028, #11259 ) ) ;
#22220 = EDGE_CURVE ( 'NONE', #12189, #22554, #21853, .T. ) ;
#22221 = CARTESIAN_POINT ( 'NONE',  ( 12.90877429640450380, 187.4316901411805816, 322.9359145523081338 ) ) ;
#22222 = B_SPLINE_CURVE_WITH_KNOTS ( 'NONE', 3,
 ( #1323, #11649, #18643, #8522, #19089, #20704, #18869, #3362 ),
 .UNSPECIFIED., .F., .F.,
 ( 4, 2, 2, 4 ),
 ( 0.002921158035944664000, 0.003648658618861576504, 0.004376159201778489008, 0.005831160367612253301 ),
 .UNSPECIFIED. ) ;
#22223 = EDGE_CURVE ( 'NONE', #13316, #6274, #4415, .T. ) ;
#22224 = CARTESIAN_POINT ( 'NONE',  ( 51.00051314569309824, 169.5754971982215125, -77.66445426478755110 ) ) ;
#22225 = CARTESIAN_POINT ( 'NONE',  ( 18.98968904741751729, 147.7994345178613287, 278.2549083691532701 ) ) ;
#22226 = CARTESIAN_POINT ( 'NONE',  ( 15.11311956079721774, 186.4324701009672367, 322.6509164249751507 ) ) ;
#22227 = EDGE_CURVE ( 'NONE', #5718, #20004, #12952, .T. ) ;
#22228 = EDGE_CURVE ( 'NONE', #20787, #13165, #7000, .T. ) ;
#22229 = LINE ( 'NONE', #18810, #9904 ) ;
#22230 = EDGE_LOOP ( 'NONE', ( #16213, #9533, #19983, #7045 ) ) ;
#22231 = CARTESIAN_POINT ( 'NONE',  ( 14.23860045627323601, 113.7412214381086670, 134.4314584438239706 ) ) ;
#22232 = CIRCLE ( 'NONE', #12376, 3.399999999999986144 ) ;
#22233 = ORIENTED_EDGE ( 'NONE', *, *, #13685, .F. ) ;
#22234 = CARTESIAN_POINT ( 'NONE',  ( 0.4135725409484927173, 69.99999999999998579, 31.99732735328655053 ) ) ;
#22235 = FACE_OUTER_BOUND ( 'NONE', #19848, .T. ) ;
#22236 = CARTESIAN_POINT ( 'NONE',  ( 11.97803979754709403, 143.5698177053941436, 275.2396454285085383 ) ) ;
#22237 = CARTESIAN_POINT ( 'NONE',  ( -11.40735840365379339, 183.0524750669035541, 320.8439791889440471 ) ) ;
#22238 = CARTESIAN_POINT ( 'NONE',  ( -9.208521424040398529, 186.6689402014612824, 307.7212088717959659 ) ) ;
#22239 = EDGE_CURVE ( 'NONE', #10097, #13377, #11557, .T. ) ;
#22240 = DIRECTION ( 'NONE',  ( 0.9726991065672934145, 0.2316562896908731239, -0.01384960395994897300 ) ) ;
#22241 = EDGE_CURVE ( 'NONE', #18285, #17745, #13069, .T. ) ;
#22242 = DIRECTION ( 'NONE',  ( 0.8909995034498461308, 2.656742962652179567E-22, 0.4540042784513463880 ) ) ;
#22243 = AXIS2_PLACEMENT_3D ( 'NONE', #2744, #2845, #20299 ) ;
#22244 = CYLINDRICAL_SURFACE ( 'NONE', #19875, 2.000000000000001332 ) ;
#22245 = EDGE_CURVE ( 'NONE', #20077, #15063, #16633, .T. ) ;
#22246 = SHAPE_DEFINITION_REPRESENTATION ( #21992, #17373 ) ;
#22247 = ORIENTED_EDGE ( 'NONE', *, *, #19002, .F. ) ;
#22248 = CARTESIAN_POINT ( 'NONE',  ( -50.94500546255758167, 109.1391869842444322, -43.51035759812305059 ) ) ;
#22249 = CARTESIAN_POINT ( 'NONE',  ( 13.06622344554902249, 190.2899467973469427, 320.8482495152294405 ) ) ;
#22250 = CARTESIAN_POINT ( 'NONE',  ( -1.163172771417702700, 81.99999999999998579, -89.99248318111824574 ) ) ;
#22251 = DIRECTION ( 'NONE',  ( 0.01035335185279153900, 0.005513005182355262476, 0.9999312050732647172 ) ) ;
#22252 = ADVANCED_FACE ( 'NONE', ( #20138 ), #5150, .T. ) ;
#22253 = CARTESIAN_POINT ( 'NONE',  ( -154.0000000000000000, 20.00000000000000000, 53.76161406891259986 ) ) ;
#22254 = LINE ( 'NONE', #6657, #7103 ) ;
#22255 = ORIENTED_EDGE ( 'NONE', *, *, #2325, .F. ) ;
#22256 = EDGE_CURVE ( 'NONE', #7056, #17777, #6271, .T. ) ;
#22257 = CARTESIAN_POINT ( 'NONE',  ( 34.11225069749755079, 94.37751527644310556, -83.07029434066950557 ) ) ;
#22258 = ORIENTED_EDGE ( 'NONE', *, *, #10949, .T. ) ;
#22259 = DIRECTION ( 'NONE',  ( 0.01292394549866739996, 0.005513023399721131770, 0.9999012842304692006 ) ) ;
#22260 = CARTESIAN_POINT ( 'NONE',  ( -40.86170866251428180, 168.8134312302532862, 57.38904148829276863 ) ) ;
#22261 = CARTESIAN_POINT ( 'NONE',  ( 106.1519489938926029, 71.09828217887417168, 28.84036442345823303 ) ) ;
#22262 = CARTESIAN_POINT ( 'NONE',  ( -5.929909278051286314, 87.00000000000001421, -93.63641280122985222 ) ) ;
#22263 = CIRCLE ( 'NONE', #2485, 2.999999999999988898 ) ;
#22264 = FACE_OUTER_BOUND ( 'NONE', #2742, .T. ) ;
#22265 = CARTESIAN_POINT ( 'NONE',  ( -50.81429207968029971, 114.2314643215460279, 169.7817148450803586 ) ) ;
#22266 = EDGE_LOOP ( 'NONE', ( #2865, #4231, #18242, #3411 ) ) ;
#22267 = DIRECTION ( 'NONE',  ( 0.000000000000000000, 1.000000000000000000, -0.000000000000000000 ) ) ;
#22268 = CYLINDRICAL_SURFACE ( 'NONE', #8494, 7.921742784567028295 ) ;
#22269 = ORIENTED_EDGE ( 'NONE', *, *, #17103, .T. ) ;
#22270 = EDGE_CURVE ( 'NONE', #8292, #9740, #4731, .T. ) ;
#22271 = AXIS2_PLACEMENT_3D ( 'NONE', #10130, #11628, #15087 ) ;
#22272 = LINE ( 'NONE', #13581, #8386 ) ;
#22273 = CARTESIAN_POINT ( 'NONE',  ( -88.16376355711264523, 88.29301322969513421, 52.88806878750047247 ) ) ;
#22274 = ADVANCED_FACE ( 'NONE', ( #3256 ), #19459, .F. ) ;
#22275 = VERTEX_POINT ( 'NONE', #21974 ) ;
#22276 = CONICAL_SURFACE ( 'NONE', #5792, 3.047499999999988329, 1.047197551196594523 ) ;
#22277 = APPLICATION_CONTEXT ( 'automotive_design' ) ;
#22278 = DIRECTION ( 'NONE',  ( -0.01292394549866745720, -0.005513023399720816918, -0.9999012842304692006 ) ) ;
#22279 = CARTESIAN_POINT ( 'NONE',  ( -34.02129075419646398, 93.60252210245951687, 83.02806418447188719 ) ) ;
#22280 = FACE_OUTER_BOUND ( 'NONE', #20645, .T. ) ;
#22281 = PRESENTATION_STYLE_ASSIGNMENT (( #10482 ) ) ;
#22282 = CARTESIAN_POINT ( 'NONE',  ( -1.362186893977295590E-13, 1.999999999999998224, 9.999999999999994671 ) ) ;
#22283 = EDGE_CURVE ( 'NONE', #4020, #9497, #4748, .T. ) ;
#22284 = CARTESIAN_POINT ( 'NONE',  ( -51.43203027167875518, 189.4933473607019607, -91.29769442758977505 ) ) ;
#22285 = ADVANCED_FACE ( 'NONE', ( #10068 ), #9830, .T. ) ;
#22286 = ORIENTED_EDGE ( 'NONE', *, *, #8992, .T. ) ;
#22287 = CARTESIAN_POINT ( 'NONE',  ( 65.90110554552376243, 105.0000000000000000, 69.29678410920483600 ) ) ;
#22288 = CARTESIAN_POINT ( 'NONE',  ( 9.785202419441143107, 190.0604574230576702, 274.9118766335186024 ) ) ;
#22289 = CARTESIAN_POINT ( 'NONE',  ( 58.13167081004702652, 143.2710928180444796, 48.49959442800331999 ) ) ;
#22290 = CARTESIAN_POINT ( 'NONE',  ( 1.364374644014609697E-14, 69.99999999999998579, -9.836443712999143722E-15 ) ) ;
#22291 = CIRCLE ( 'NONE', #16092, 3.047499999999998987 ) ;
#22292 = CARTESIAN_POINT ( 'NONE',  ( -11.65206543345498602, 147.5984083283656787, 277.2097828948077449 ) ) ;
#22293 = DIRECTION ( 'NONE',  ( -0.000000000000000000, -1.000000000000000000, 0.000000000000000000 ) ) ;
#22294 = CIRCLE ( 'NONE', #6545, 2.000000000000001332 ) ;
#22295 = CARTESIAN_POINT ( 'NONE',  ( 13.07910534688314819, 160.8951497186004076, 323.8457538311976123 ) ) ;
#22296 = VERTEX_POINT ( 'NONE', #9945 ) ;
#22297 = CARTESIAN_POINT ( 'NONE',  ( -10.23725882687554112, 186.5193182284470197, 276.8889396700154748 ) ) ;
#22298 = ORIENTED_EDGE ( 'NONE', *, *, #18395, .F. ) ;
#22299 = DIRECTION ( 'NONE',  ( -0.01292414190463832269, 0.000000000000000000, -0.9999164797902017066 ) ) ;
#22300 = EDGE_CURVE ( 'NONE', #4942, #20544, #4979, .T. ) ;
#22301 = EDGE_CURVE ( 'NONE', #9954, #7572, #11907, .T. ) ;
#22302 = VECTOR ( 'NONE', #16485, 1000.000000000000000 ) ;
#22303 = ORIENTED_EDGE ( 'NONE', *, *, #14765, .F. ) ;
#22304 = CARTESIAN_POINT ( 'NONE',  ( -34.79726985247908999, 121.2962013336460956, 248.0347590154626971 ) ) ;
#22305 = LINE ( 'NONE', #1106, #7425 ) ;
#22306 = CARTESIAN_POINT ( 'NONE',  ( 86.21288355311105533, 75.00269236436724896, -0.2926965463156551706 ) ) ;
#22307 = FACE_OUTER_BOUND ( 'NONE', #8216, .T. ) ;
#22308 = CARTESIAN_POINT ( 'NONE',  ( 12.81503532323078964, 190.4972571607467842, 307.8483445055002221 ) ) ;
#22309 = CYLINDRICAL_SURFACE ( 'NONE', #7685, 2.999999999999988898 ) ;
#22310 = CARTESIAN_POINT ( 'NONE',  ( 52.91240873130399081, 106.8060942374655156, 70.25530070199208410 ) ) ;
#22311 = DIRECTION ( 'NONE',  ( -0.01292394549866740169, -0.005513023399721131770, -0.9999012842304693116 ) ) ;
#22312 = CARTESIAN_POINT ( 'NONE',  ( 13.80637996605699769, 137.5572120012638777, 100.9913744321402902 ) ) ;
#22314 = CARTESIAN_POINT ( 'NONE',  ( 0.000000000000000000, 0.000000000000000000, 0.000000000000000000 ) ) ;
#22313 = B_SPLINE_CURVE_WITH_KNOTS ( 'NONE', 3,
 ( #17149, #4718, #5059, #15228, #18863, #1203, #18638, #17054, #3127, #18968, #22284, #11643, #1317, #6690, #8197, #1421 ),
 .UNSPECIFIED., .F., .F.,
 ( 4, 2, 2, 2, 2, 2, 2, 4 ),
 ( 6.938893903907228378E-18, 0.0003951465896843917307, 0.0007902931793687765225, 0.001185439769053161152, 0.001580586358737546106, 0.002370879538106300186, 0.002766026127790658252, 0.003161172717475016318 ),
 .UNSPECIFIED. ) ;
#22315 = VERTEX_POINT ( 'NONE', #22310 ) ;
#22316 = CARTESIAN_POINT ( 'NONE',  ( -41.58451242677338655, 92.58578643762699301, -83.88377541325537834 ) ) ;
#22317 = ORIENTED_EDGE ( 'NONE', *, *, #8390, .T. ) ;
#22318 = AXIS2_PLACEMENT_3D ( 'NONE', #1011, #18351, #21876 ) ;
#22319 = VERTEX_POINT ( 'NONE', #4867 ) ;
#22320 = DIRECTION ( 'NONE',  ( -2.025474946048326158E-22, 1.000000000000000000, -1.876735158486678933E-22 ) ) ;
#22321 = LINE ( 'NONE', #20837, #18384 ) ;
#22322 = VERTEX_POINT ( 'NONE', #6275 ) ;
#22323 = CARTESIAN_POINT ( 'NONE',  ( -66.42308629463825298, 169.3906321239456361, -109.6814500331617381 ) ) ;
#22324 = ORIENTED_EDGE ( 'NONE', *, *, #13962, .F. ) ;
#22325 = EDGE_CURVE ( 'NONE', #7542, #3218, #22516, .T. ) ;
#22326 = DIRECTION ( 'NONE',  ( -0.01292394549866744159, -0.005513023399721009472, -0.9999012842304692006 ) ) ;
#22327 = ORIENTED_EDGE ( 'NONE', *, *, #9855, .F. ) ;
#22328 = DIRECTION ( 'NONE',  ( -0.9999164797902015955, 0.000000000000000000, 0.01292414190464162733 ) ) ;
#22329 = AXIS2_PLACEMENT_3D ( 'NONE', #11534, #18535, #11640 ) ;
#22330 = CARTESIAN_POINT ( 'NONE',  ( -1.163172771417702478, 87.00000000000001421, -89.99248318111824574 ) ) ;
#22331 = CARTESIAN_POINT ( 'NONE',  ( 18.54079482392480926, 146.0746420647028003, 276.2612673939528918 ) ) ;
#22332 = ORIENTED_EDGE ( 'NONE', *, *, #496, .T. ) ;
#22333 = VECTOR ( 'NONE', #692, 1000.000000000000114 ) ;
#22334 = CARTESIAN_POINT ( 'NONE',  ( -9.107733615807006800, 30.00000000000000711, -96.06569921463757566 ) ) ;
#22335 = LINE ( 'NONE', #17327, #3663 ) ;
#22336 = FACE_OUTER_BOUND ( 'NONE', #19588, .T. ) ;
#22337 = LINE ( 'NONE', #17329, #6411 ) ;
#22338 = ORIENTED_EDGE ( 'NONE', *, *, #14483, .F. ) ;
#22339 = DIRECTION ( 'NONE',  ( 1.000000000000000000, 0.000000000000000000, -1.387778780781444413E-14 ) ) ;
#22340 = DIRECTION ( 'NONE',  ( 0.01292394549866727679, 0.005513023399720742325, 0.9999012842304692006 ) ) ;
#22341 = DIRECTION ( 'NONE',  ( -0.9999164797902017066, -6.965998958219365988E-18, 0.01292414190464157356 ) ) ;
#22342 = CONICAL_SURFACE ( 'NONE', #6950, 24.99999999999998224, 0.03490658503988662564 ) ;
#22343 = AXIS2_PLACEMENT_3D ( 'NONE', #20339, #6776, #13468 ) ;
#22344 = CARTESIAN_POINT ( 'NONE',  ( -56.89103422957282419, 143.2573102595449654, 47.48611753646095224 ) ) ;
#22345 = AXIS2_PLACEMENT_3D ( 'NONE', #2305, #9180, #5629 ) ;
#22346 = CARTESIAN_POINT ( 'NONE',  ( -7.774884586432870393, 70.00000000000002842, -96.16248895089307780 ) ) ;
#22347 = EDGE_CURVE ( 'NONE', #3063, #19220, #15456, .T. ) ;
#22348 = CARTESIAN_POINT ( 'NONE',  ( -41.67747345744908216, 165.9786531560170886, 257.1849355913342379 ) ) ;
#22349 = CARTESIAN_POINT ( 'NONE',  ( 92.05960170301050027, 69.99999999999998579, -60.20821982323567312 ) ) ;
#22350 = TOROIDAL_SURFACE ( 'NONE', #6966, 83.00000000000001421, 2.000000000000000000 ) ;
#22351 = APPLICATION_PROTOCOL_DEFINITION ( 'draft international standard', 'automotive_design', 1998, #8949 ) ;
#22352 = VERTEX_POINT ( 'NONE', #20490 ) ;
#22353 = CARTESIAN_POINT ( 'NONE',  ( -38.46706438352714486, 91.17157287525387233, 85.27439087629285552 ) ) ;
#22354 = DIRECTION ( 'NONE',  ( 0.01292394549866624984, 0.005513023399719273882, 0.9999012842304693116 ) ) ;
#22355 = DIRECTION ( 'NONE',  ( 0.01292414190464131508, 0.000000000000000000, 0.9999164797902017066 ) ) ;
#22356 = DIRECTION ( 'NONE',  ( 5.440186201345738641E-18, 1.000000000000000000, 1.334940939666364181E-17 ) ) ;
#22357 = CARTESIAN_POINT ( 'NONE',  ( -48.80698602204240188, 140.5066718483590762, 92.62435808135882098 ) ) ;
#22358 = AXIS2_PLACEMENT_3D ( 'NONE', #1898, #1783, #9233 ) ;
#22359 = FACE_OUTER_BOUND ( 'NONE', #12425, .T. ) ;
#22360 = CARTESIAN_POINT ( 'NONE',  ( 163.9999999999998863, 2.000000000000000000, -8.000000000002268408 ) ) ;
#22361 = EDGE_CURVE ( 'NONE', #15351, #5229, #2529, .T. ) ;
#22362 = ORIENTED_EDGE ( 'NONE', *, *, #10689, .F. ) ;
#22363 = CARTESIAN_POINT ( 'NONE',  ( -90.11270991033710231, 87.45691446470777919, 51.12027952437478717 ) ) ;
#22364 = ORIENTED_EDGE ( 'NONE', *, *, #21858, .F. ) ;
#22365 = CARTESIAN_POINT ( 'NONE',  ( 161.9999999999992610, 18.00000000000000355, -53.76161406891482386 ) ) ;
#22366 = EDGE_CURVE ( 'NONE', #2469, #19973, #11791, .T. ) ;
#22367 = AXIS2_PLACEMENT_3D ( 'NONE', #17573, #3951, #19795 ) ;
#22368 = DIRECTION ( 'NONE',  ( 0.9999164797902017066, 2.001050586450178931E-22, -0.01292414190464131508 ) ) ;
#22369 = CARTESIAN_POINT ( 'NONE',  ( 163.9999999999998863, 1.999999999999998224, -8.000000000002268408 ) ) ;
#22370 = DIRECTION ( 'NONE',  ( -0.000000000000000000, -1.000000000000000000, -0.000000000000000000 ) ) ;
#22371 = EDGE_CURVE ( 'NONE', #10181, #19868, #13610, .T. ) ;
#22372 = ORIENTED_EDGE ( 'NONE', *, *, #22167, .T. ) ;
#22373 = FACE_OUTER_BOUND ( 'NONE', #17794, .T. ) ;
#22374 = DIRECTION ( 'NONE',  ( 0.8981428216242032248, -6.500054012300580894E-17, -0.4397038457472424167 ) ) ;
#22375 = AXIS2_PLACEMENT_3D ( 'NONE', #17535, #9236, #16288 ) ;
#22376 = VERTEX_POINT ( 'NONE', #21152 ) ;
#22377 = FACE_OUTER_BOUND ( 'NONE', #20885, .T. ) ;
#22378 = DIRECTION ( 'NONE',  ( -0.01292394549866747802, -0.005513023399721269681, -0.9999012842304692006 ) ) ;
#22379 = VERTEX_POINT ( 'NONE', #14175 ) ;
#22380 = EDGE_CURVE ( 'NONE', #4461, #5296, #5641, .T. ) ;
#22381 = PLANE ( 'NONE',  #16489 ) ;
#22382 = VECTOR ( 'NONE', #13162, 999.9999999999998863 ) ;
#22383 = CARTESIAN_POINT ( 'NONE',  ( -88.16473883906751041, 88.38724588659185599, 52.80379687237449815 ) ) ;
#22384 = EDGE_CURVE ( 'NONE', #1394, #9371, #18184, .T. ) ;
#22385 = AXIS2_PLACEMENT_3D ( 'NONE', #4359, #14751, #21701 ) ;
#22386 = AXIS2_PLACEMENT_3D ( 'NONE', #10152, #1428, #3232 ) ;
#22387 = EDGE_CURVE ( 'NONE', #17220, #8554, #2537, .T. ) ;
#22389 = ORIENTED_EDGE ( 'NONE', *, *, #2047, .T. ) ;
#22388 = ORIENTED_EDGE ( 'NONE', *, *, #20441, .T. ) ;
#22390 = CARTESIAN_POINT ( 'NONE',  ( -74.93579704394247187, 95.43814120535131451, 80.52726847798278698 ) ) ;
#22391 = CIRCLE ( 'NONE', #15835, 24.99999999999998224 ) ;
#22392 = CARTESIAN_POINT ( 'NONE',  ( 39.36913080622081651, 69.99999999999998579, -87.51612159803863733 ) ) ;
#22393 = CARTESIAN_POINT ( 'NONE',  ( -22.89256597249752545, 88.79858284056908246, -77.57367698057866789 ) ) ;
#22394 =( NAMED_UNIT ( * ) SI_UNIT ( $, .STERADIAN. ) SOLID_ANGLE_UNIT ( ) );
#22395 = CARTESIAN_POINT ( 'NONE',  ( 5.149300590115022835, 70.80384757729338219, -98.24794683011701579 ) ) ;
#22396 = LINE ( 'NONE', #11411, #8561 ) ;
#22397 = CARTESIAN_POINT ( 'NONE',  ( -71.18985671402974447, 92.11167198312699611, -83.85708946072359993 ) ) ;
#22398 = ADVANCED_FACE ( 'NONE', ( #2092, #2436 ), #21252, .T. ) ;
#22399 = ORIENTED_EDGE ( 'NONE', *, *, #17694, .F. ) ;
#22400 = EDGE_LOOP ( 'NONE', ( #8346, #4746 ) ) ;
#22401 = ORIENTED_EDGE ( 'NONE', *, *, #4262, .T. ) ;
#22402 = CARTESIAN_POINT ( 'NONE',  ( -55.34016076973275489, 143.9188730675114414, 167.4742716441172377 ) ) ;
#22403 = CARTESIAN_POINT ( 'NONE',  ( 0.000000000000000000, 23.00000000000000000, 0.000000000000000000 ) ) ;
#22404 = LINE ( 'NONE', #22188, #7598 ) ;
#22405 = CARTESIAN_POINT ( 'NONE',  ( -90.03465221005033925, 70.01281497139055432, 63.19621350536183968 ) ) ;
#22406 = AXIS2_PLACEMENT_3D ( 'NONE', #19557, #9088, #268 ) ;
#22407 = CARTESIAN_POINT ( 'NONE',  ( -2.067862704742604141, 69.99999999999998579, -159.9866367664322979 ) ) ;
#22408 = EDGE_CURVE ( 'NONE', #11384, #3194, #5399, .T. ) ;
#22409 = ORIENTED_EDGE ( 'NONE', *, *, #4970, .F. ) ;
#22410 = SHAPE_REPRESENTATION_RELATIONSHIP ( 'NONE' , 'NONE' ,  #7092, #4147 ) ;
#22411 = CARTESIAN_POINT ( 'NONE',  ( -56.08207636726148593, 126.6021325681200551, 110.0736613710297007 ) ) ;
#22412 = CIRCLE ( 'NONE', #8475, 22.49999999999999645 ) ;
#22413 = CIRCLE ( 'NONE', #21329, 112.5000000000000284 ) ;
#22414 = CARTESIAN_POINT ( 'NONE',  ( -64.00442900045042904, 100.0478588994083964, 77.44550239952441473 ) ) ;
#22415 = ORIENTED_EDGE ( 'NONE', *, *, #19705, .F. ) ;
#22416 = ORIENTED_EDGE ( 'NONE', *, *, #16953, .F. ) ;
#22417 = FACE_OUTER_BOUND ( 'NONE', #22134, .T. ) ;
#22418 = ADVANCED_FACE ( 'NONE', ( #8973 ), #3812, .F. ) ;
#22419 = CIRCLE ( 'NONE', #19132, 110.5324305509042233 ) ;
#22420 = VERTEX_POINT ( 'NONE', #15904 ) ;
#22421 = AXIS2_PLACEMENT_3D ( 'NONE', #5116, #19138, #3416 ) ;
#22422 = DIRECTION ( 'NONE',  ( 0.01292394549866738608, 0.005513023399720699824, 0.9999012842304692006 ) ) ;
#22423 = CARTESIAN_POINT ( 'NONE',  ( -90.22705529645503475, 71.16332133347465572, 60.80384032246523418 ) ) ;
#22424 = VECTOR ( 'NONE', #7020, 999.9999999999998863 ) ;
#22425 = CARTESIAN_POINT ( 'NONE',  ( 39.45066905836480942, 123.7663955596447352, -42.75919236024152070 ) ) ;
#22426 = DIRECTION ( 'NONE',  ( -1.372099599554306628E-14, 0.000000000000000000, 1.000000000000000000 ) ) ;
#22427 = VECTOR ( 'NONE', #4130, 1000.000000000000114 ) ;
#22428 = CARTESIAN_POINT ( 'NONE',  ( 54.52327687265658085, 0.000000000000000000, -111.3697098814019171 ) ) ;
#22429 = DIRECTION ( 'NONE',  ( 0.1296504907605110779, 0.005475273188902231650, 0.9915446392518419971 ) ) ;
#22430 = CARTESIAN_POINT ( 'NONE',  ( 49.99582398951009310, 170.0000000000008242, -0.6462070952312342076 ) ) ;
#22431 = DIRECTION ( 'NONE',  ( 0.01292414190464174703, 0.000000000000000000, 0.9999164797902015955 ) ) ;
#22432 = CARTESIAN_POINT ( 'NONE',  ( -51.99565694909051672, 170.0000000000000284, 0.6720553790413400508 ) ) ;
#22433 = CARTESIAN_POINT ( 'NONE',  ( -51.20141213521757351, 189.5954075083848238, -72.78685549352853457 ) ) ;
#22434 = PLANE ( 'NONE',  #14333 ) ;
#22435 = EDGE_CURVE ( 'NONE', #16857, #22201, #8805, .T. ) ;
#22436 =( BOUNDED_CURVE ( )  B_SPLINE_CURVE ( 3, ( #17331, #1588, #5237, #19141 ),
 .UNSPECIFIED., .F., .T. ) 
 B_SPLINE_CURVE_WITH_KNOTS ( ( 4, 4 ),
 ( 0.4472747960204455087, 0.4841788640348455020 ),
 .UNSPECIFIED. ) 
 CURVE ( )  GEOMETRIC_REPRESENTATION_ITEM ( )  RATIONAL_B_SPLINE_CURVE ( ( 1.000000000000000000, 0.9998865107004337727, 0.9998865107004337727, 1.000000000000000000 ) ) 
 REPRESENTATION_ITEM ( '' )  );
#22437 = AXIS2_PLACEMENT_3D ( 'NONE', #20535, #6868, #17464 ) ;
#22438 = CIRCLE ( 'NONE', #10731, 1.999999999999997780 ) ;
#22439 = CARTESIAN_POINT ( 'NONE',  ( -40.33104288128404846, 94.48610424851698042, 83.91830964824988826 ) ) ;
#22440 = DIRECTION ( 'NONE',  ( -0.01292394549866750231, -0.005513023399722823126, -0.9999012842304692006 ) ) ;
#22441 = ORIENTED_EDGE ( 'NONE', *, *, #22132, .T. ) ;
#22442 = DIRECTION ( 'NONE',  ( 0.01292394549866733230, 0.005513023399720419666, 0.9999012842304692006 ) ) ;
#22443 = EDGE_LOOP ( 'NONE', ( #10901, #614, #619, #5810, #5543 ) ) ;
#22444 = EDGE_CURVE ( 'NONE', #19328, #10450, #4139, .T. ) ;
#22445 = CARTESIAN_POINT ( 'NONE',  ( -7.475646132950445555, 70.80384757729335377, -81.73701953211951832 ) ) ;
#22446 = CARTESIAN_POINT ( 'NONE',  ( -5.731715098087014404, 326.6288426432528240, 307.3396573775339107 ) ) ;
#22447 = CARTESIAN_POINT ( 'NONE',  ( -10.85980368455889433, 163.6991139211620236, 126.9796742121690443 ) ) ;
#22448 = ORIENTED_EDGE ( 'NONE', *, *, #2258, .T. ) ;
#22449 = CARTESIAN_POINT ( 'NONE',  ( 12.62120397054262710, 187.5429183231100012, 322.9525087504210887 ) ) ;
#22450 = DIRECTION ( 'NONE',  ( 0.01292394549866738782, 0.005513023399720701559, 0.9999012842304693116 ) ) ;
#22451 = EDGE_CURVE ( 'NONE', #16920, #15659, #7148, .T. ) ;
#22452 = FACE_OUTER_BOUND ( 'NONE', #9135, .T. ) ;
#22453 = EDGE_CURVE ( 'NONE', #13100, #17793, #12972, .T. ) ;
#22454 = DIRECTION ( 'NONE',  ( 7.125109674081160920E-05, -0.9999848031710253382, 0.005512562950849312846 ) ) ;
#22455 = ORIENTED_EDGE ( 'NONE', *, *, #16123, .T. ) ;
#22456 = DIRECTION ( 'NONE',  ( -0.01292394549866737914, -0.005513023399721009472, -0.9999012842304692006 ) ) ;
#22457 = LINE ( 'NONE', #6748, #2589 ) ;
#22458 = DIRECTION ( 'NONE',  ( 0.9999164797902017066, 0.000000000000000000, -0.01292414190463751951 ) ) ;
#22459 = AXIS2_PLACEMENT_3D ( 'NONE', #17193, #1466, #4999 ) ;
#22460 = CYLINDRICAL_SURFACE ( 'NONE', #14689, 3.399999999999985700 ) ;
#22461 = DIRECTION ( 'NONE',  ( 0.2126763768167733992, 0.9770888199431678744, -0.008136134595576589509 ) ) ;
#22462 = ORIENTED_EDGE ( 'NONE', *, *, #15315, .T. ) ;
#22463 = DIRECTION ( 'NONE',  ( -2.025474946048326158E-22, 1.000000000000000000, -1.876735158486679638E-22 ) ) ;
#22464 = DIRECTION ( 'NONE',  ( 0.009760756503427210282, -0.9999378516499566327, 0.005387065077606872227 ) ) ;
#22465 = CARTESIAN_POINT ( 'NONE',  ( -17.35589273022797485, 113.6997816401180472, 127.3226006773067525 ) ) ;
#22466 = ITEM_DEFINED_TRANSFORMATION ( 'NONE', 'NONE', #1486,  #6292 ) ;
#22467 = AXIS2_PLACEMENT_3D ( 'NONE', #13954, #180, #19230 ) ;
#22468 = EDGE_LOOP ( 'NONE', ( #17405, #6424, #16528, #1688 ) ) ;
#22469 = CARTESIAN_POINT ( 'NONE',  ( -42.64951291394369548, 126.1473081376431367, 27.39440536439884255 ) ) ;
#22470 = CARTESIAN_POINT ( 'NONE',  ( 44.31784132852413194, 168.2105890667581605, -53.06813496338226344 ) ) ;
#22471 = DIRECTION ( 'NONE',  ( 0.01292394549866737220, 0.005513023399721000799, 0.9999012842304692006 ) ) ;
#22472 = CARTESIAN_POINT ( 'NONE',  ( -14.52969038923042966, 137.6261247937603969, 113.8584785293034400 ) ) ;
#22473 = ORIENTED_EDGE ( 'NONE', *, *, #14588, .T. ) ;
#22474 = TOROIDAL_SURFACE ( 'NONE', #22124, 118.0000000000000000, 2.000000000000000000 ) ;
#22475 = ORIENTED_EDGE ( 'NONE', *, *, #12077, .F. ) ;
#22476 = CARTESIAN_POINT ( 'NONE',  ( -4.006862498311197562, 172.5094284590153393, 324.6687400670222701 ) ) ;
#22477 = AXIS2_PLACEMENT_3D ( 'NONE', #6927, #17415, #20944 ) ;
#22478 = CARTESIAN_POINT ( 'NONE',  ( -48.58807999359533625, 108.9796592258344390, -43.53994181459253099 ) ) ;
#22479 = EDGE_CURVE ( 'NONE', #19234, #9818, #788, .T. ) ;
#22480 = ORIENTED_EDGE ( 'NONE', *, *, #13782, .T. ) ;
#22481 = VERTEX_POINT ( 'NONE', #10832 ) ;
#22482 = CARTESIAN_POINT ( 'NONE',  ( -87.76353177753581747, 103.0887459898907821, -66.33296338796036196 ) ) ;
#22483 = LINE ( 'NONE', #18724, #21184 ) ;
#22484 = CARTESIAN_POINT ( 'NONE',  ( 48.82059446874842479, 189.4989811950858609, -91.57149822991706856 ) ) ;
#22485 = DIRECTION ( 'NONE',  ( -7.125109674364536131E-05, 0.9999848031710253382, -0.005512562950849706628 ) ) ;
#22486 = AXIS2_PLACEMENT_3D ( 'NONE', #10588, #5063, #14281 ) ;
#22487 = ORIENTED_EDGE ( 'NONE', *, *, #10107, .T. ) ;
#22488 = CARTESIAN_POINT ( 'NONE',  ( -13.50073983619024531, 183.7065926015648074, 278.6553669534395681 ) ) ;
#22489 = CARTESIAN_POINT ( 'NONE',  ( -90.00000000000000000, 29.00000000000000355, 8.394090934816448357E-16 ) ) ;
#22490 = ORIENTED_EDGE ( 'NONE', *, *, #13061, .F. ) ;
#22491 = VECTOR ( 'NONE', #21431, 1000.000000000000114 ) ;
#22492 = VECTOR ( 'NONE', #9571, 1000.000000000000114 ) ;
#22493 = CARTESIAN_POINT ( 'NONE',  ( 90.21557837424575155, 71.13279352004266798, -62.93780832164412686 ) ) ;
#22494 = ADVANCED_FACE ( 'NONE', ( #12677 ), #10935, .T. ) ;
#22495 = CARTESIAN_POINT ( 'NONE',  ( -90.07292945398545214, 88.55600042780055503, 52.68328250211072827 ) ) ;
#22496 = ORIENTED_EDGE ( 'NONE', *, *, #14121, .T. ) ;
#22497 = EDGE_LOOP ( 'NONE', ( #7166, #14247, #6670, #11954 ) ) ;
#22498 = DIRECTION ( 'NONE',  ( 0.9999164797902015955, 2.001050586498092550E-22, -0.01292414190464117457 ) ) ;
#22499 = DIRECTION ( 'NONE',  ( -0.9909299940865188283, 0.1338359446631172955, 0.01207007604876741101 ) ) ;
#22500 = DIRECTION ( 'NONE',  ( -0.9934404589540162256, -0.1135548637187059617, 0.01346653032742970747 ) ) ;
#22501 = ORIENTED_EDGE ( 'NONE', *, *, #12315, .F. ) ;
#22502 = VECTOR ( 'NONE', #21346, 1000.000000000000114 ) ;
#22503 = CARTESIAN_POINT ( 'NONE',  ( 80.05923150692980528, 75.13699351169597662, 4.065642694558706083 ) ) ;
#22504 = DIRECTION ( 'NONE',  ( 7.125109674364534776E-05, -0.9999848031710252272, 0.005512562950849704893 ) ) ;
#22505 = EDGE_LOOP ( 'NONE', ( #19710, #20624, #9580, #9142, #13753 ) ) ;
#22506 = ORIENTED_EDGE ( 'NONE', *, *, #16709, .F. ) ;
#22507 = CARTESIAN_POINT ( 'NONE',  ( -2.096375399687102625, 190.2200455327031818, 274.6112675210154634 ) ) ;
#22508 = DIRECTION ( 'NONE',  ( 0.01292414190464131508, 0.000000000000000000, 0.9999164797902017066 ) ) ;
#22509 = DIRECTION ( 'NONE',  ( -0.008205354412248759208, 0.7726059781012496464, -0.6348327927582039232 ) ) ;
#22510 = CARTESIAN_POINT ( 'NONE',  ( -40.33104288128404846, 94.48610424851698042, 83.91830964824988826 ) ) ;
#22511 = EDGE_CURVE ( 'NONE', #18283, #3170, #10319, .T. ) ;
#22512 = CIRCLE ( 'NONE', #11554, 2.000000000000006661 ) ;
#22513 = ADVANCED_FACE ( 'NONE', ( #21481 ), #16575, .F. ) ;
#22514 = CARTESIAN_POINT ( 'NONE',  ( -12.73793622217206156, 148.6298842822529878, 278.8389053497636496 ) ) ;
#22515 = SURFACE_STYLE_USAGE ( .BOTH. , #13724 ) ;
#22516 = B_SPLINE_CURVE_WITH_KNOTS ( 'NONE', 3,
 ( #16974, #8427, #6501, #13301, #16850, #17297, #1111, #10167, #8108, #22091, #6394, #8322, #18664, #17178 ),
 .UNSPECIFIED., .F., .F.,
 ( 4, 2, 2, 2, 2, 2, 4 ),
 ( 0.000000000000000000, 0.0003927847099521207183, 0.0007855694199042414366, 0.001178354129856362155, 0.001571138839808482873, 0.002356708259712697422, 0.003142277679616911536 ),
 .UNSPECIFIED. ) ;
#22517 = DIRECTION ( 'NONE',  ( 0.1296504907605108559, 0.005475273188901296634, 0.9915446392518419971 ) ) ;
#22518 = VERTEX_POINT ( 'NONE', #7362 ) ;
#22519 = AXIS2_PLACEMENT_3D ( 'NONE', #2442, #4146, #2328 ) ;
#22520 = ORIENTED_EDGE ( 'NONE', *, *, #17744, .T. ) ;
#22521 = ORIENTED_EDGE ( 'NONE', *, *, #7546, .T. ) ;
#22522 = UNCERTAINTY_MEASURE_WITH_UNIT (LENGTH_MEASURE( 1.000000000000000082E-05 ), #5775, 'distance_accuracy_value', 'NONE');
#22523 = EDGE_CURVE ( 'NONE', #16185, #11013, #6211, .T. ) ;
#22524 = LINE ( 'NONE', #18654, #20321 ) ;
#22525 = EDGE_CURVE ( 'NONE', #11778, #17346, #22157, .T. ) ;
#22527 = ORIENTED_EDGE ( 'NONE', *, *, #19929, .F. ) ;
#22526 = ORIENTED_EDGE ( 'NONE', *, *, #4431, .T. ) ;
#22528 = ADVANCED_FACE ( 'NONE', ( #11724 ), #2666, .T. ) ;
#22529 = CARTESIAN_POINT ( 'NONE',  ( -49.10926328453583523, 107.8891387851018635, 70.20563931596009866 ) ) ;
#22530 = CARTESIAN_POINT ( 'NONE',  ( -89.87368547071935154, 72.07415593028026990, 62.10066946404283783 ) ) ;
#22531 = DIRECTION ( 'NONE',  ( -0.7944560844389300103, 0.000000000000000000, -0.6073216033519338586 ) ) ;
#22532 = DIRECTION ( 'NONE',  ( 0.000000000000000000, 1.000000000000000000, 0.000000000000000000 ) ) ;
#22533 = SURFACE_STYLE_USAGE ( .BOTH. , #8543 ) ;
#22534 = CARTESIAN_POINT ( 'NONE',  ( -19.00623411919002592, 140.4227465520235967, 77.01503843080352851 ) ) ;
#22535 = CARTESIAN_POINT ( 'NONE',  ( 11.80168056336799687, 187.7948655116154555, 307.7666879900542085 ) ) ;
#22536 = CARTESIAN_POINT ( 'NONE',  ( -40.58168163415708563, 127.0293918815982011, 187.3786108412739395 ) ) ;
#22537 = EDGE_CURVE ( 'NONE', #10132, #15344, #20053, .T. ) ;
#22538 = DIRECTION ( 'NONE',  ( 0.009188991635466048358, -0.7031977391749438810, 0.7109349492407661675 ) ) ;
#22539 = CARTESIAN_POINT ( 'NONE',  ( -41.96503124479402658, 165.8559883853732515, 234.9371320172060678 ) ) ;
#22540 = DIRECTION ( 'NONE',  ( 0.000000000000000000, 0.000000000000000000, 1.000000000000000000 ) ) ;
#22541 = DIRECTION ( 'NONE',  ( 0.6074180324222079319, 7.300068142772960434E-18, -0.7943823600057678957 ) ) ;
#22542 = VERTEX_POINT ( 'NONE', #21919 ) ;
#22543 = CARTESIAN_POINT ( 'NONE',  ( -91.24493283426484425, 78.25381457448439448, -30.56897831620035788 ) ) ;
#22544 = VERTEX_POINT ( 'NONE', #9425 ) ;
#22545 = VECTOR ( 'NONE', #6092, 999.9999999999998863 ) ;
#22546 = FACE_OUTER_BOUND ( 'NONE', #15767, .T. ) ;
#22547 = B_SPLINE_CURVE_WITH_KNOTS ( 'NONE', 3,
 ( #12725, #18013, #3865, #10641, #10876, #14226 ),
 .UNSPECIFIED., .F., .F.,
 ( 4, 2, 4 ),
 ( 0.005030677301327409964, 0.006487126694169642084, 0.007943576087011874204 ),
 .UNSPECIFIED. ) ;
#22548 = ADVANCED_FACE ( 'NONE', ( #16908 ), #22036, .F. ) ;
#22549 = PRODUCT_DEFINITION_CONTEXT ( 'detailed design', #11311, 'design' ) ;
#22550 = PLANE ( 'NONE',  #22459 ) ;
#22551 = CARTESIAN_POINT ( 'NONE',  ( -12.86548928906161571, 326.2291019854885121, 410.4442357137708086 ) ) ;
#22552 = VERTEX_POINT ( 'NONE', #13465 ) ;
#22553 = CARTESIAN_POINT ( 'NONE',  ( 89.66113247980437961, 100.6041916471017856, 63.72504470331089266 ) ) ;
#22554 = VERTEX_POINT ( 'NONE', #16585 ) ;
#22555 = CARTESIAN_POINT ( 'NONE',  ( 13.76115603162017820, 155.5381941787832716, 97.49248393264142010 ) ) ;
#22556 = EDGE_CURVE ( 'NONE', #1880, #17838, #18399, .T. ) ;
#22557 = CARTESIAN_POINT ( 'NONE',  ( 109.5595887168318114, 75.67202325895546267, 10.09161844407532982 ) ) ;
#22558 = CARTESIAN_POINT ( 'NONE',  ( 1.163172771417732010, 69.99999999999998579, 89.99248318111813205 ) ) ;
#22559 = DIRECTION ( 'NONE',  ( -0.01292394549866740863, -0.005513023399721009472, -0.9999012842304692006 ) ) ;
#22560 = EDGE_LOOP ( 'NONE', ( #4740, #19446, #19583, #11538 ) ) ;
#22561 = CARTESIAN_POINT ( 'NONE',  ( 106.1636641531657972, 79.04398536104962147, -28.79715981783310497 ) ) ;
#22562 = CARTESIAN_POINT ( 'NONE',  ( 163.9999999999998863, 18.00000000000000355, -8.000000000002268408 ) ) ;
#22563 = CARTESIAN_POINT ( 'NONE',  ( -75.90743353164272378, 96.21294322789842113, -79.81268430165903283 ) ) ;
#22564 = LINE ( 'NONE', #3083, #10298 ) ;
#22565 = APPLICATION_CONTEXT ( 'automotive_design' ) ;
#22566 = CARTESIAN_POINT ( 'NONE',  ( 19.77615078807425064, 182.9145900011216668, 318.4299545691768003 ) ) ;
#22567 = CARTESIAN_POINT ( 'NONE',  ( 35.39322062607229213, 92.77591188308413450, -83.66707218845637328 ) ) ;
#22568 = DIRECTION ( 'NONE',  ( -7.125109674160325297E-05, 0.9999848031710253382, -0.005512562950849327591 ) ) ;
#22569 = CARTESIAN_POINT ( 'NONE',  ( -1.163172771417702700, 69.99999999999998579, -89.99248318111824574 ) ) ;
#22570 = CARTESIAN_POINT ( 'NONE',  ( -1.163172771417702700, 81.97459999999998104, -89.99248318111824574 ) ) ;
#22571 = ADVANCED_FACE ( 'NONE', ( #4254 ), #4691, .T. ) ;
#22572 = CONTEXT_DEPENDENT_SHAPE_REPRESENTATION ( #3239, #13970 ) ;
#22573 = ADVANCED_FACE ( 'NONE', ( #19987 ), #2776, .T. ) ;
#22574 = CARTESIAN_POINT ( 'NONE',  ( 27.86414599017677673, -5.346239964818102486, -10.69171401565444235 ) ) ;
#22576 = ORIENTED_EDGE ( 'NONE', *, *, #11871, .T. ) ;
#22575 = ORIENTED_EDGE ( 'NONE', *, *, #10206, .T. ) ;
#22577 = CARTESIAN_POINT ( 'NONE',  ( -164.0000000000000000, 1.999999999999998224, 8.000000000000019540 ) ) ;
#22578 = CARTESIAN_POINT ( 'NONE',  ( 68.43148148480361215, 69.99999999999998579, 86.12277481476651531 ) ) ;
#22579 = DIRECTION ( 'NONE',  ( -0.01292394549866743465, -0.005513023399721021615, -0.9999012842304692006 ) ) ;
#22580 = DIRECTION ( 'NONE',  ( -0.7161863329816247070, -0.003898296230782349273, -0.6978982302147144212 ) ) ;
#22581 = AXIS2_PLACEMENT_3D ( 'NONE', #2771, #22029, #22149 ) ;
#22582 = ORIENTED_EDGE ( 'NONE', *, *, #10191, .T. ) ;
#22583 = CARTESIAN_POINT ( 'NONE',  ( -1.432836755002403442E-14, 25.00000000000000000, -117.0000000000000000 ) ) ;
#22584 = CARTESIAN_POINT ( 'NONE',  ( -48.90524865575625313, 110.4369068636443671, -43.54387697287747727 ) ) ;
#22585 = ORIENTED_EDGE ( 'NONE', *, *, #5205, .F. ) ;
#22586 = CARTESIAN_POINT ( 'NONE',  ( -89.07320425719680657, 88.54727852611058836, 50.44093601027914531 ) ) ;
#22587 = EDGE_LOOP ( 'NONE', ( #1282, #3809, #2360, #1350 ) ) ;
#22588 = SHAPE_REPRESENTATION_RELATIONSHIP ( 'NONE' , 'NONE' ,  #10922, #19533 ) ;
#22589 = CARTESIAN_POINT ( 'NONE',  ( 106.2142196127746132, 77.44923501812733946, 28.61015647369538684 ) ) ;
#22590 = DIRECTION ( 'NONE',  ( 0.9232306267972777425, 0.000000000000000000, -0.3842462878721221164 ) ) ;
#22591 = CARTESIAN_POINT ( 'NONE',  ( 40.65822637310714782, 91.17157287525387233, 84.25167897319538213 ) ) ;
#22592 = DIRECTION ( 'NONE',  ( 0.01292394549866740169, 0.005513023399720822990, 0.9999012842304693116 ) ) ;
#22593 = SURFACE_STYLE_USAGE ( .BOTH. , #20899 ) ;
#22594 = CARTESIAN_POINT ( 'NONE',  ( 3.394697517040290435, 158.4152025170260742, 256.6430692997608389 ) ) ;
#22595 = ORIENTED_EDGE ( 'NONE', *, *, #8341, .F. ) ;
#22596 = CARTESIAN_POINT ( 'NONE',  ( 21.04327404614685193, 168.6617636117169070, 311.0793389543180751 ) ) ;
#22597 = ORIENTED_EDGE ( 'NONE', *, *, #20196, .T. ) ;
#22598 = LINE ( 'NONE', #10575, #332 ) ;
#22599 = ADVANCED_FACE ( 'NONE', ( #9784 ), #13359, .T. ) ;
#22600 = CARTESIAN_POINT ( 'NONE',  ( -89.96085446817751574, 87.79024195230550731, 50.91569201083114393 ) ) ;
#22601 = CARTESIAN_POINT ( 'NONE',  ( 73.74384038452764401, 74.99999999999998579, -0.9531554654672949045 ) ) ;
#22602 = ORIENTED_EDGE ( 'NONE', *, *, #14314, .T. ) ;
#22603 = VERTEX_POINT ( 'NONE', #13124 ) ;
#22604 = FACE_OUTER_BOUND ( 'NONE', #7998, .T. ) ;
#22605 = CARTESIAN_POINT ( 'NONE',  ( 0.000000000000000000, 18.00000000000000355, -126.0000000000000000 ) ) ;
#22606 = DIRECTION ( 'NONE',  ( 0.009138748381789112835, -0.7071067811865462405, 0.7070477234798342447 ) ) ;
#22607 = FILL_AREA_STYLE ('',( #3223 ) ) ;
#22608 = CARTESIAN_POINT ( 'NONE',  ( 84.66884248357162335, 75.02317907734844482, 1.009935179570716546 ) ) ;
#22609 = VECTOR ( 'NONE', #19989, 999.9999999999998863 ) ;
#22610 = FACE_BOUND ( 'NONE', #10573, .T. ) ;
#22611 = VERTEX_POINT ( 'NONE', #713 ) ;
#22612 = EDGE_LOOP ( 'NONE', ( #10843, #6968, #4900, #13969 ) ) ;
#22613 = CARTESIAN_POINT ( 'NONE',  ( -65.62836707099317834, 91.01435578462051978, 67.50627132372665073 ) ) ;
#22614 = CARTESIAN_POINT ( 'NONE',  ( 65.34011313256004883, 145.1470193978928478, 25.89385934263124867 ) ) ;
#22615 = CARTESIAN_POINT ( 'NONE',  ( 16.33911976870347971, 185.7005718863503319, 320.1529740037655642 ) ) ;
#22616 = CARTESIAN_POINT ( 'NONE',  ( -26.82015259287494402, 324.2622591174701938, 318.5097988702426619 ) ) ;
#22617 = FACE_OUTER_BOUND ( 'NONE', #11735, .T. ) ;
#22618 = VERTEX_POINT ( 'NONE', #15201 ) ;
#22619 = DIRECTION ( 'NONE',  ( -0.004263634442766561783, 0.9440169652124852373, -0.3298693541575938859 ) ) ;
#22620 = DIRECTION ( 'NONE',  ( 0.01292394549866738782, 0.005513023399720468239, 0.9999012842304692006 ) ) ;
#22621 = DIRECTION ( 'NONE',  ( 1.396592535537253658E-14, -0.000000000000000000, 1.000000000000000000 ) ) ;
#22622 = VERTEX_POINT ( 'NONE', #18286 ) ;
#22623 = ORIENTED_EDGE ( 'NONE', *, *, #12885, .F. ) ;
#22624 = AXIS2_PLACEMENT_3D ( 'NONE', #17588, #13902, #14028 ) ;
#22625 = DIRECTION ( 'NONE',  ( 2.025474946048326158E-22, -1.000000000000000000, 1.876735158486679638E-22 ) ) ;
#22626 = EDGE_CURVE ( 'NONE', #8399, #14240, #16797, .T. ) ;
#22627 = ORIENTED_EDGE ( 'NONE', *, *, #3930, .F. ) ;
#22628 = CARTESIAN_POINT ( 'NONE',  ( 65.44350469654938252, 145.1911235850906223, 33.89306961647502447 ) ) ;
#22629 = CARTESIAN_POINT ( 'NONE',  ( -90.41395131934733342, 70.35743632279135795, 62.65252801945162275 ) ) ;
#22630 = ADVANCED_FACE ( 'NONE', ( #835 ), #8041, .F. ) ;
#22631 = CONICAL_SURFACE ( 'NONE', #15356, 4.999999999999990230, 1.047197551196595855 ) ;
#22632 = FACE_OUTER_BOUND ( 'NONE', #2267, .T. ) ;
#22633 = CARTESIAN_POINT ( 'NONE',  ( -38.91888847133742502, 97.29933205984647770, 83.90205325766430633 ) ) ;
#22634 = FACE_OUTER_BOUND ( 'NONE', #10179, .T. ) ;
#22635 = CARTESIAN_POINT ( 'NONE',  ( 85.88862024204405543, 75.02104826936582072, -3.119601652154077254 ) ) ;
#22636 = CARTESIAN_POINT ( 'NONE',  ( 12.82301040887749188, 190.4942272971743478, 307.8488580778642358 ) ) ;
#22637 = CARTESIAN_POINT ( 'NONE',  ( 10.15309714582121714, 176.0218267656414355, 323.4662548820142547 ) ) ;
#22638 = ORIENTED_EDGE ( 'NONE', *, *, #20293, .F. ) ;
#22639 = ADVANCED_FACE ( 'NONE', ( #21807 ), #14740, .F. ) ;
#22640 = DIRECTION ( 'NONE',  ( 0.01292414190464131682, 0.000000000000000000, 0.9999164797902017066 ) ) ;
#22641 = ORIENTED_EDGE ( 'NONE', *, *, #17372, .F. ) ;
#22642 = EDGE_CURVE ( 'NONE', #4308, #15481, #12913, .T. ) ;
#22643 = CARTESIAN_POINT ( 'NONE',  ( -56.92334409331949274, 143.2435277010456787, 44.98636432588477874 ) ) ;
#22644 = CARTESIAN_POINT ( 'NONE',  ( -10.07221555630028220, 187.8236846762713981, 308.1657108960777691 ) ) ;
#22645 = ORIENTED_EDGE ( 'NONE', *, *, #6175, .F. ) ;
#22646 = CARTESIAN_POINT ( 'NONE',  ( -4.264070500929974195, 189.5987719431177538, 275.3263399216110088 ) ) ;
#22647 = AXIS2_PLACEMENT_3D ( 'NONE', #13065, #14668, #4520 ) ;
#22648 = ORIENTED_EDGE ( 'NONE', *, *, #12705, .T. ) ;
#22649 = AXIS2_PLACEMENT_3D ( 'NONE', #10703, #8726, #7142 ) ;
#22650 =( GEOMETRIC_REPRESENTATION_CONTEXT ( 3 ) GLOBAL_UNCERTAINTY_ASSIGNED_CONTEXT ( ( #5313 ) ) GLOBAL_UNIT_ASSIGNED_CONTEXT ( ( #15714, #12265, #2947 ) ) REPRESENTATION_CONTEXT ( 'NONE', 'WORKASPACE' ) );
#22651 = ADVANCED_FACE ( 'NONE', ( #6339 ), #4594, .F. ) ;
#22652 = CARTESIAN_POINT ( 'NONE',  ( -8.330024601187750122, 185.3742117612894447, 323.2535488253523681 ) ) ;
#22653 = EDGE_CURVE ( 'NONE', #11172, #8011, #17664, .T. ) ;
#22654 = CARTESIAN_POINT ( 'NONE',  ( -26.94222022802838268, 95.51270090492249665, 82.01937116434972097 ) ) ;
#22655 = EDGE_CURVE ( 'NONE', #15997, #19048, #16220, .T. ) ;
#22656 = ADVANCED_FACE ( 'NONE', ( #15310 ), #6662, .F. ) ;
#22657 = DIRECTION ( 'NONE',  ( 0.01292394549866743465, 0.005513023399721021615, 0.9999012842304692006 ) ) ;
#22658 = CARTESIAN_POINT ( 'NONE',  ( -10.92070568566948197, 73.91464330287723783, 120.9748739040315968 ) ) ;
#22659 = CARTESIAN_POINT ( 'NONE',  ( 11.28650372074689834, 143.4152113759959377, 275.6042146768694465 ) ) ;
#22660 = ORIENTED_EDGE ( 'NONE', *, *, #3050, .T. ) ;
#22661 = CARTESIAN_POINT ( 'NONE',  ( 14.08796030271276045, 105.6768406389637107, 122.7767139219343164 ) ) ;
#22662 = ORIENTED_EDGE ( 'NONE', *, *, #2894, .T. ) ;
#22663 = EDGE_LOOP ( 'NONE', ( #5814, #22324, #12767, #6046 ) ) ;
#22664 = DIRECTION ( 'NONE',  ( 0.01292394549866738608, 0.005513023399720698957, 0.9999012842304692006 ) ) ;
#22665 = AXIS2_PLACEMENT_3D ( 'NONE', #5231, #12274, #19258 ) ;
#22666 = NEXT_ASSEMBLY_USAGE_OCCURRENCE ( 'NAUO1', ' ', ' ', #9450, #7492, $ ) ;
#22667 = NEXT_ASSEMBLY_USAGE_OCCURRENCE ( 'NAUO2', ' ', ' ', #9450, #12273, $ ) ;
#22668 = NEXT_ASSEMBLY_USAGE_OCCURRENCE ( 'NAUO3', ' ', ' ', #9450, #21773, $ ) ;
#22669 = NEXT_ASSEMBLY_USAGE_OCCURRENCE ( 'NAUO4', ' ', ' ', #9450, #18443, $ ) ;
#22670 = NEXT_ASSEMBLY_USAGE_OCCURRENCE ( 'NAUO5', ' ', ' ', #9450, #15651, $ ) ;
#22671 = NEXT_ASSEMBLY_USAGE_OCCURRENCE ( 'NAUO6', ' ', ' ', #9450, #1029, $ ) ;
#22672 = NEXT_ASSEMBLY_USAGE_OCCURRENCE ( 'NAUO7', ' ', ' ', #9450, #20803, $ ) ;
#22673 = NEXT_ASSEMBLY_USAGE_OCCURRENCE ( 'NAUO8', ' ', ' ', #9450, #18701, $ ) ;
#22674 = NEXT_ASSEMBLY_USAGE_OCCURRENCE ( 'NAUO9', ' ', ' ', #9450, #5782, $ ) ;
#22675 = NEXT_ASSEMBLY_USAGE_OCCURRENCE ( 'NAUO10', ' ', ' ', #9450, #9870, $ ) ;
#22676 = NEXT_ASSEMBLY_USAGE_OCCURRENCE ( 'NAUO11', ' ', ' ', #9450, #7900, $ ) ;
#22677 = NEXT_ASSEMBLY_USAGE_OCCURRENCE ( 'NAUO12', ' ', ' ', #9450, #2728, $ ) ;
#22678 = NEXT_ASSEMBLY_USAGE_OCCURRENCE ( 'NAUO13', ' ', ' ', #9450, #20389, $ ) ;
#22679 = NEXT_ASSEMBLY_USAGE_OCCURRENCE ( 'NAUO14', ' ', ' ', #9450, #9157, $ ) ;
#22680 = NEXT_ASSEMBLY_USAGE_OCCURRENCE ( 'NAUO15', ' ', ' ', #9450, #2137, $ ) ;
#22681 = NEXT_ASSEMBLY_USAGE_OCCURRENCE ( 'NAUO16', ' ', ' ', #9450, #13264, $ ) ;
#22682 = NEXT_ASSEMBLY_USAGE_OCCURRENCE ( 'NAUO17', ' ', ' ', #9450, #13947, $ ) ;
#22683 = NEXT_ASSEMBLY_USAGE_OCCURRENCE ( 'NAUO18', ' ', ' ', #9450, #13947, $ ) ;
#22684 = NEXT_ASSEMBLY_USAGE_OCCURRENCE ( 'NAUO19', ' ', ' ', #9450, #13264, $ ) ;
#22685 = NEXT_ASSEMBLY_USAGE_OCCURRENCE ( 'NAUO20', ' ', ' ', #9450, #15651, $ ) ;
#22686 = NEXT_ASSEMBLY_USAGE_OCCURRENCE ( 'NAUO21', ' ', ' ', #9450, #7900, $ ) ;
#22687 = NEXT_ASSEMBLY_USAGE_OCCURRENCE ( 'NAUO22', ' ', ' ', #9450, #18701, $ ) ;
#22688 = NEXT_ASSEMBLY_USAGE_OCCURRENCE ( 'NAUO23', ' ', ' ', #9450, #21773, $ ) ;
#22689 = NEXT_ASSEMBLY_USAGE_OCCURRENCE ( 'NAUO24', ' ', ' ', #9450, #9870, $ ) ;
#22690 = NEXT_ASSEMBLY_USAGE_OCCURRENCE ( 'NAUO25', ' ', ' ', #9450, #5782, $ ) ;
#22691 = NEXT_ASSEMBLY_USAGE_OCCURRENCE ( 'NAUO26', ' ', ' ', #9450, #2728, $ ) ;
#22692 = NEXT_ASSEMBLY_USAGE_OCCURRENCE ( 'NAUO27', ' ', ' ', #9450, #15651, $ ) ;
#22693 = NEXT_ASSEMBLY_USAGE_OCCURRENCE ( 'NAUO28', ' ', ' ', #9450, #15651, $ ) ;
#22694 = NEXT_ASSEMBLY_USAGE_OCCURRENCE ( 'NAUO29', ' ', ' ', #9450, #15651, $ ) ;
#22695 = NEXT_ASSEMBLY_USAGE_OCCURRENCE ( 'NAUO30', ' ', ' ', #9450, #15651, $ ) ;
#22696 = NEXT_ASSEMBLY_USAGE_OCCURRENCE ( 'NAUO31', ' ', ' ', #9450, #21773, $ ) ;
#22697 = NEXT_ASSEMBLY_USAGE_OCCURRENCE ( 'NAUO32', ' ', ' ', #9450, #21773, $ ) ;
#22698 = NEXT_ASSEMBLY_USAGE_OCCURRENCE ( 'NAUO33', ' ', ' ', #9450, #21773, $ ) ;
#22699 = NEXT_ASSEMBLY_USAGE_OCCURRENCE ( 'NAUO34', ' ', ' ', #9450, #21773, $ ) ;
#22700 = NEXT_ASSEMBLY_USAGE_OCCURRENCE ( 'NAUO35', ' ', ' ', #9450, #13264, $ ) ;
#22701 = NEXT_ASSEMBLY_USAGE_OCCURRENCE ( 'NAUO36', ' ', ' ', #9450, #13264, $ ) ;
ENDSEC;
END-ISO-10303-21;
